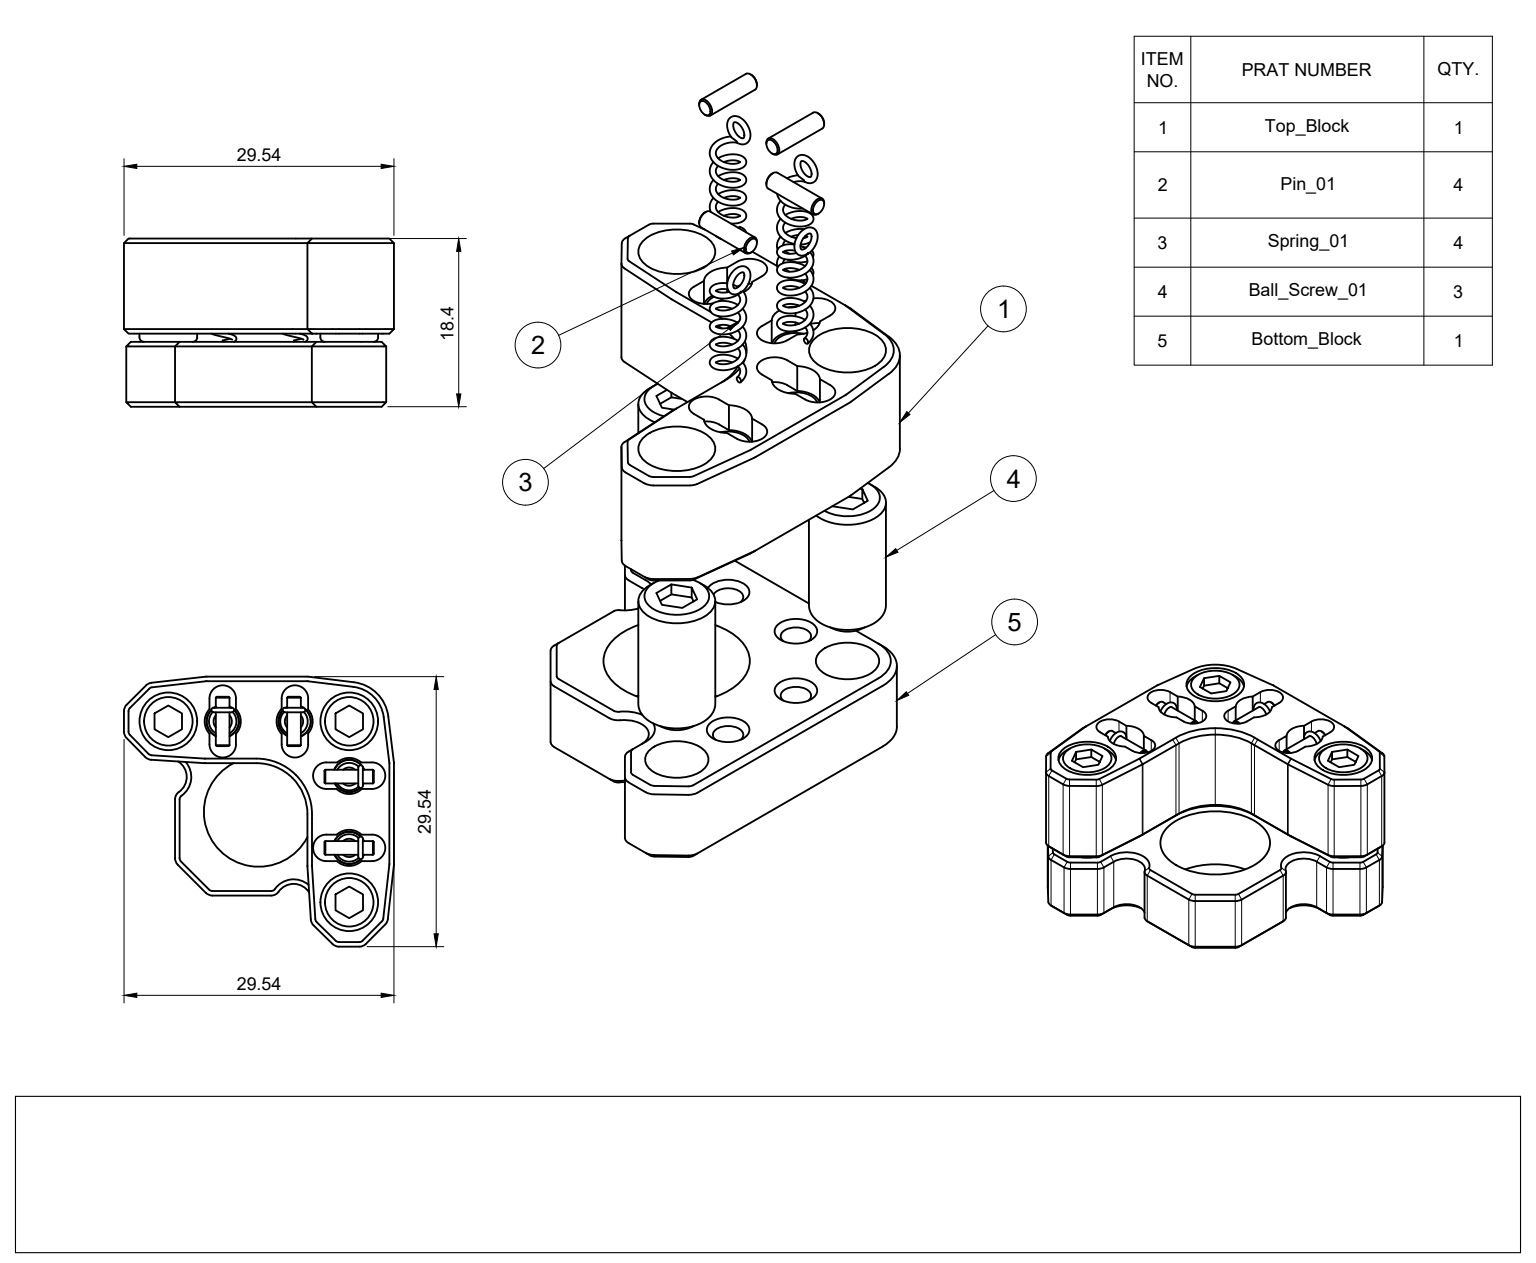
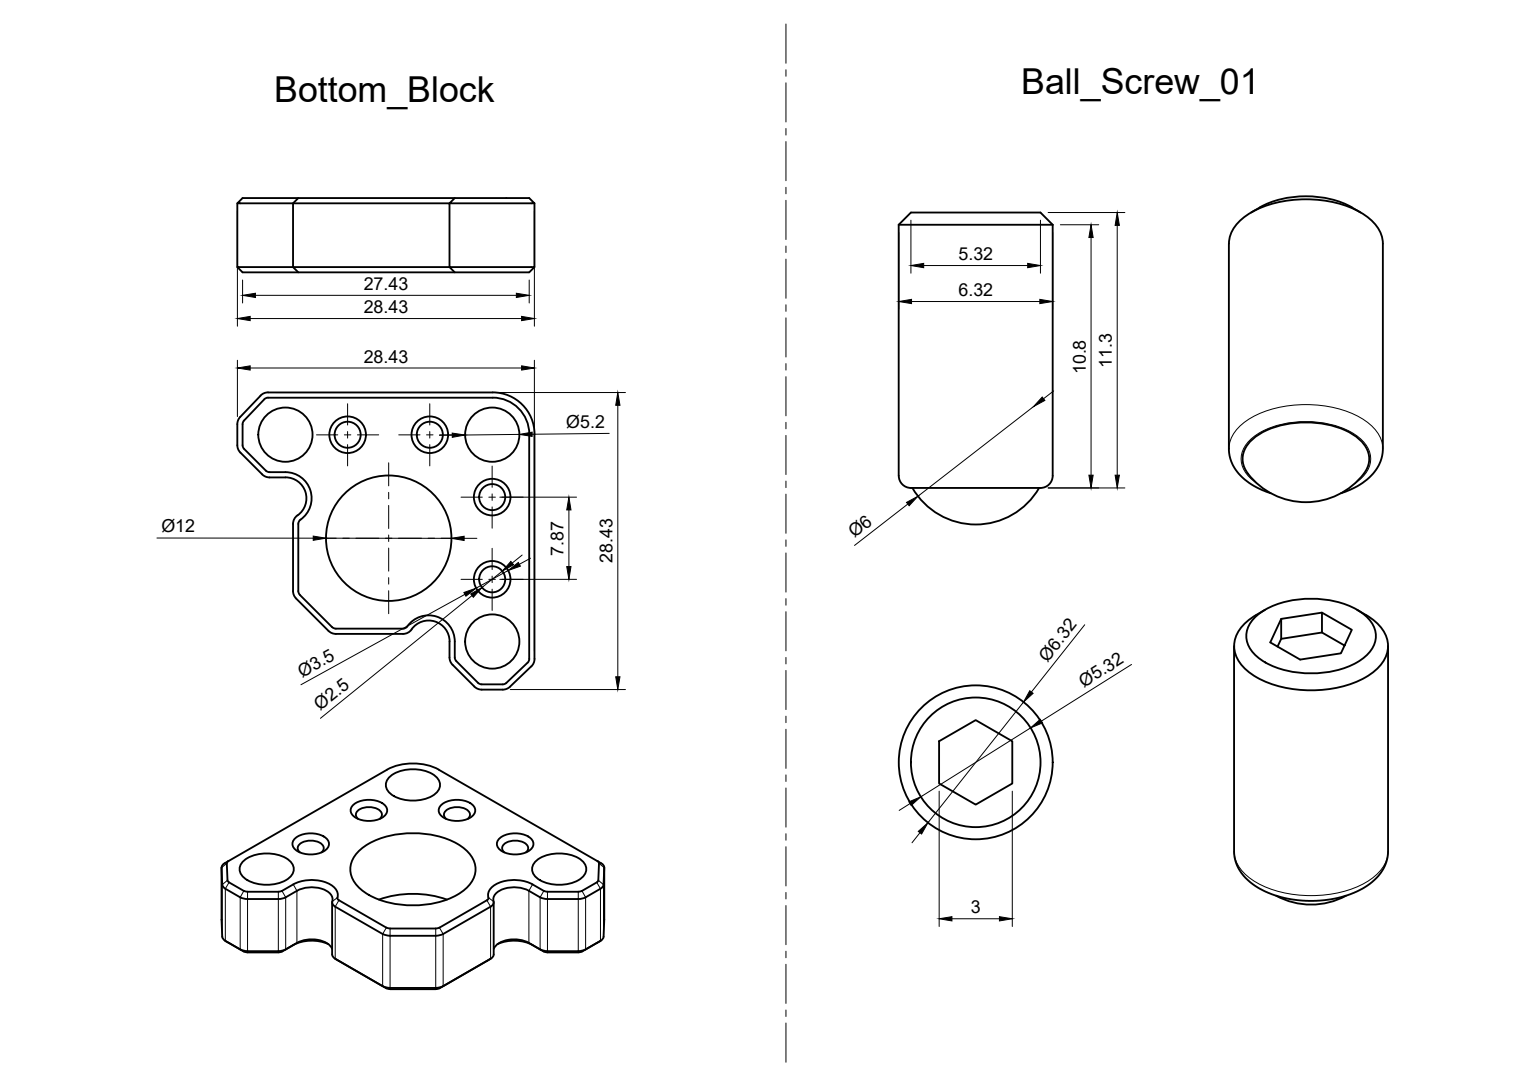
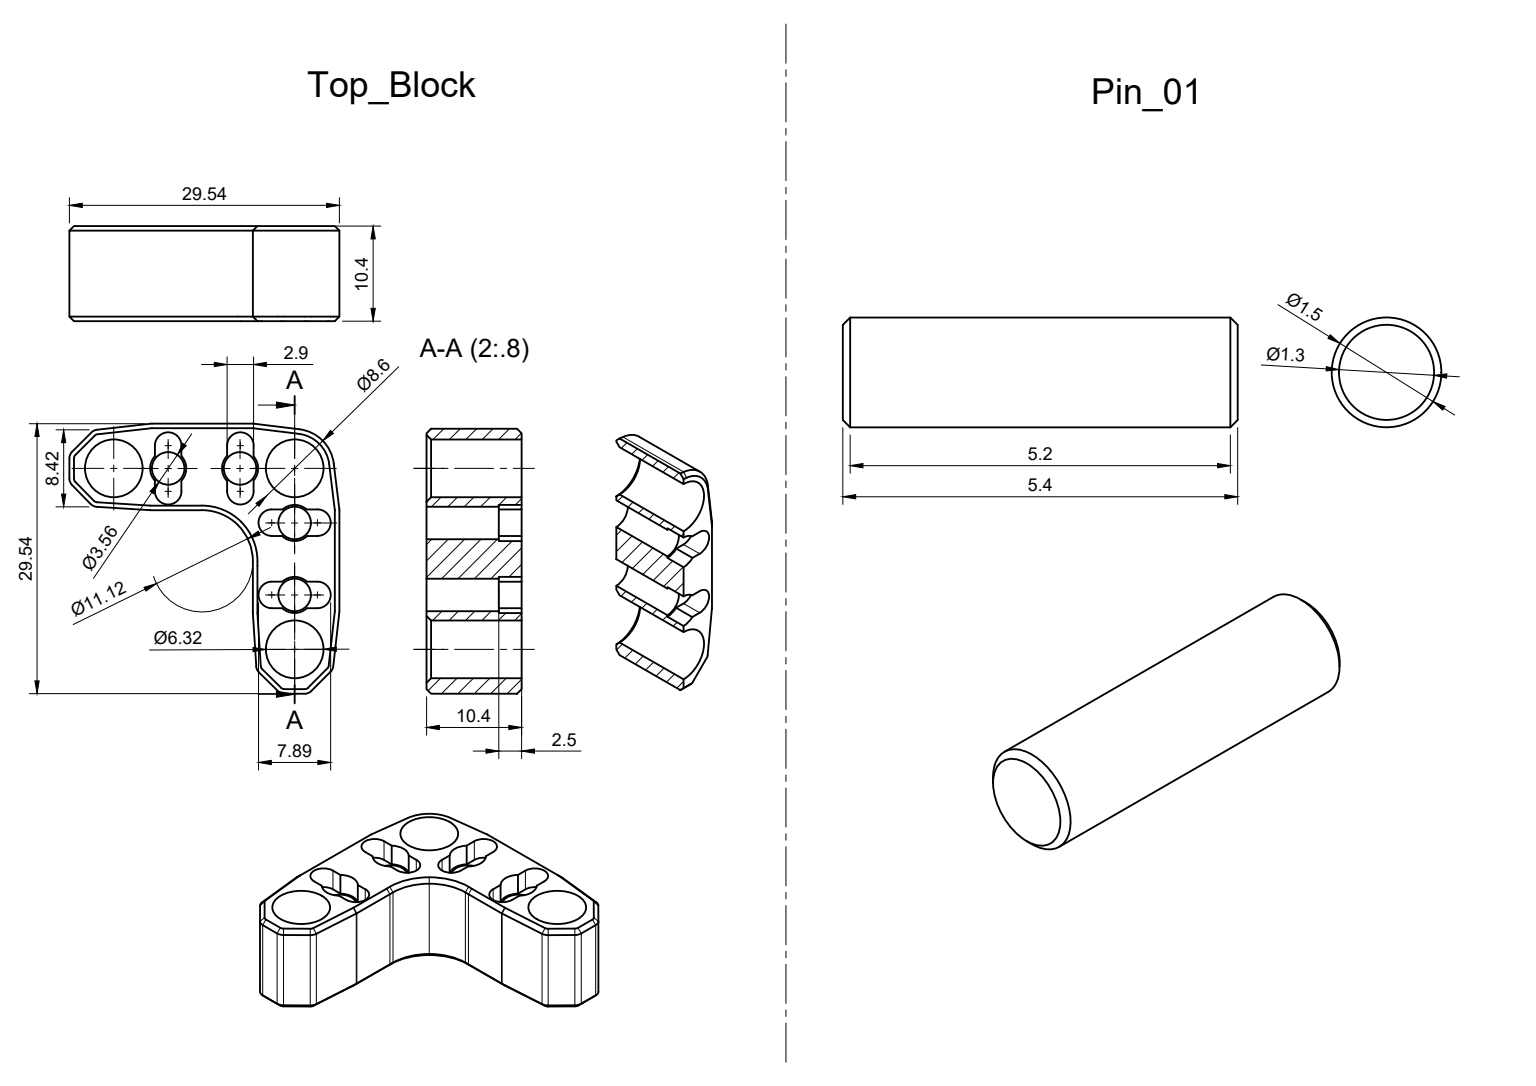
ISO-10303-21;
HEADER;
/* Generated by software containing ST-Developer
 * from STEP Tools, Inc. (www.steptools.com) 
 */

FILE_DESCRIPTION(
/* description */ (''),
/* implementation_level */ '2;1');

FILE_NAME(
/* name */ 'MAS-280',
/* time_stamp */ '2026-10-23T17:00:58+06:00',
/* author */ (''),
/* organization */ (''),
/* preprocessor_version */ 'ST-DEVELOPER v20.2',
/* originating_system */ 'Autodesk Translation Framework v15.15.0.0',
/* authorisation */ '');

FILE_SCHEMA (('AUTOMOTIVE_DESIGN { 1 0 10303 214 3 1 1 }'));
ENDSEC;

DATA;
#10=MECHANICAL_DESIGN_GEOMETRIC_PRESENTATION_REPRESENTATION('',(#106,#107,
#108,#109,#110,#111,#112,#113,#114,#115,#116,#117,#118),#11385);
#11=ITEM_DEFINED_TRANSFORMATION($,$,#5500,#6097);
#12=ITEM_DEFINED_TRANSFORMATION($,$,#5779,#6098);
#13=ITEM_DEFINED_TRANSFORMATION($,$,#5789,#6099);
#14=ITEM_DEFINED_TRANSFORMATION($,$,#5796,#6100);
#15=ITEM_DEFINED_TRANSFORMATION($,$,#5817,#6101);
#16=ITEM_DEFINED_TRANSFORMATION($,$,#6004,#6102);
#17=ITEM_DEFINED_TRANSFORMATION($,$,#6014,#6103);
#18=ITEM_DEFINED_TRANSFORMATION($,$,#6035,#6104);
#19=ITEM_DEFINED_TRANSFORMATION($,$,#6042,#6105);
#20=ITEM_DEFINED_TRANSFORMATION($,$,#6049,#6106);
#21=ITEM_DEFINED_TRANSFORMATION($,$,#6059,#6107);
#22=ITEM_DEFINED_TRANSFORMATION($,$,#6066,#6108);
#23=ITEM_DEFINED_TRANSFORMATION($,$,#6076,#6109);
#24=(
REPRESENTATION_RELATIONSHIP($,$,#11432,#11431)
REPRESENTATION_RELATIONSHIP_WITH_TRANSFORMATION(#11)
SHAPE_REPRESENTATION_RELATIONSHIP()
);
#25=(
REPRESENTATION_RELATIONSHIP($,$,#11433,#11431)
REPRESENTATION_RELATIONSHIP_WITH_TRANSFORMATION(#12)
SHAPE_REPRESENTATION_RELATIONSHIP()
);
#26=(
REPRESENTATION_RELATIONSHIP($,$,#11434,#11431)
REPRESENTATION_RELATIONSHIP_WITH_TRANSFORMATION(#13)
SHAPE_REPRESENTATION_RELATIONSHIP()
);
#27=(
REPRESENTATION_RELATIONSHIP($,$,#11435,#11431)
REPRESENTATION_RELATIONSHIP_WITH_TRANSFORMATION(#14)
SHAPE_REPRESENTATION_RELATIONSHIP()
);
#28=(
REPRESENTATION_RELATIONSHIP($,$,#11436,#11431)
REPRESENTATION_RELATIONSHIP_WITH_TRANSFORMATION(#15)
SHAPE_REPRESENTATION_RELATIONSHIP()
);
#29=(
REPRESENTATION_RELATIONSHIP($,$,#11437,#11431)
REPRESENTATION_RELATIONSHIP_WITH_TRANSFORMATION(#16)
SHAPE_REPRESENTATION_RELATIONSHIP()
);
#30=(
REPRESENTATION_RELATIONSHIP($,$,#11438,#11431)
REPRESENTATION_RELATIONSHIP_WITH_TRANSFORMATION(#17)
SHAPE_REPRESENTATION_RELATIONSHIP()
);
#31=(
REPRESENTATION_RELATIONSHIP($,$,#11439,#11431)
REPRESENTATION_RELATIONSHIP_WITH_TRANSFORMATION(#18)
SHAPE_REPRESENTATION_RELATIONSHIP()
);
#32=(
REPRESENTATION_RELATIONSHIP($,$,#11440,#11431)
REPRESENTATION_RELATIONSHIP_WITH_TRANSFORMATION(#19)
SHAPE_REPRESENTATION_RELATIONSHIP()
);
#33=(
REPRESENTATION_RELATIONSHIP($,$,#11441,#11431)
REPRESENTATION_RELATIONSHIP_WITH_TRANSFORMATION(#20)
SHAPE_REPRESENTATION_RELATIONSHIP()
);
#34=(
REPRESENTATION_RELATIONSHIP($,$,#11442,#11431)
REPRESENTATION_RELATIONSHIP_WITH_TRANSFORMATION(#21)
SHAPE_REPRESENTATION_RELATIONSHIP()
);
#35=(
REPRESENTATION_RELATIONSHIP($,$,#11443,#11431)
REPRESENTATION_RELATIONSHIP_WITH_TRANSFORMATION(#22)
SHAPE_REPRESENTATION_RELATIONSHIP()
);
#36=(
REPRESENTATION_RELATIONSHIP($,$,#11444,#11431)
REPRESENTATION_RELATIONSHIP_WITH_TRANSFORMATION(#23)
SHAPE_REPRESENTATION_RELATIONSHIP()
);
#37=CONTEXT_DEPENDENT_SHAPE_REPRESENTATION(#24,#11418);
#38=CONTEXT_DEPENDENT_SHAPE_REPRESENTATION(#25,#11419);
#39=CONTEXT_DEPENDENT_SHAPE_REPRESENTATION(#26,#11420);
#40=CONTEXT_DEPENDENT_SHAPE_REPRESENTATION(#27,#11421);
#41=CONTEXT_DEPENDENT_SHAPE_REPRESENTATION(#28,#11422);
#42=CONTEXT_DEPENDENT_SHAPE_REPRESENTATION(#29,#11423);
#43=CONTEXT_DEPENDENT_SHAPE_REPRESENTATION(#30,#11424);
#44=CONTEXT_DEPENDENT_SHAPE_REPRESENTATION(#31,#11425);
#45=CONTEXT_DEPENDENT_SHAPE_REPRESENTATION(#32,#11426);
#46=CONTEXT_DEPENDENT_SHAPE_REPRESENTATION(#33,#11427);
#47=CONTEXT_DEPENDENT_SHAPE_REPRESENTATION(#34,#11428);
#48=CONTEXT_DEPENDENT_SHAPE_REPRESENTATION(#35,#11429);
#49=CONTEXT_DEPENDENT_SHAPE_REPRESENTATION(#36,#11430);
#50=NEXT_ASSEMBLY_USAGE_OCCURRENCE('Top_Block:1','Top_Block:1',
'Top_Block:1',#11446,#11447,'Top_Block:1');
#51=NEXT_ASSEMBLY_USAGE_OCCURRENCE('Pin_01:1','Pin_01:1','Pin_01:1',#11446,
#11448,'Pin_01:1');
#52=NEXT_ASSEMBLY_USAGE_OCCURRENCE('Spring_01:1','Spring_01:1',
'Spring_01:1',#11446,#11449,'Spring_01:1');
#53=NEXT_ASSEMBLY_USAGE_OCCURRENCE('Ball_Screw_01:1','Ball_Screw_01:1',
'Ball_Screw_01:1',#11446,#11450,'Ball_Screw_01:1');
#54=NEXT_ASSEMBLY_USAGE_OCCURRENCE('Bottom_Block:1','Bottom_Block:1',
'Bottom_Block:1',#11446,#11451,'Bottom_Block:1');
#55=NEXT_ASSEMBLY_USAGE_OCCURRENCE('Pin_04:1','Pin_04:1','Pin_04:1',#11446,
#11452,'Pin_04:1');
#56=NEXT_ASSEMBLY_USAGE_OCCURRENCE('Ball_Screw_02:1','Ball_Screw_02:1',
'Ball_Screw_02:1',#11446,#11453,'Ball_Screw_02:1');
#57=NEXT_ASSEMBLY_USAGE_OCCURRENCE('Spring_04:1','Spring_04:1',
'Spring_04:1',#11446,#11454,'Spring_04:1');
#58=NEXT_ASSEMBLY_USAGE_OCCURRENCE('Spring_02:1','Spring_02:1',
'Spring_02:1',#11446,#11455,'Spring_02:1');
#59=NEXT_ASSEMBLY_USAGE_OCCURRENCE('Pin_03:1','Pin_03:1','Pin_03:1',#11446,
#11456,'Pin_03:1');
#60=NEXT_ASSEMBLY_USAGE_OCCURRENCE('Spring_03:1','Spring_03:1',
'Spring_03:1',#11446,#11457,'Spring_03:1');
#61=NEXT_ASSEMBLY_USAGE_OCCURRENCE('Pin_02:1','Pin_02:1','Pin_02:1',#11446,
#11458,'Pin_02:1');
#62=NEXT_ASSEMBLY_USAGE_OCCURRENCE('Ball_Screw_03:1','Ball_Screw_03:1',
'Ball_Screw_03:1',#11446,#11459,'Ball_Screw_03:1');
#63=SPHERICAL_SURFACE('',#5797,3.);
#64=SPHERICAL_SURFACE('',#5818,3.);
#65=SPHERICAL_SURFACE('',#5844,3.);
#66=SPHERICAL_SURFACE('',#5846,3.);
#67=SPHERICAL_SURFACE('',#6015,3.);
#68=SPHERICAL_SURFACE('',#6077,3.);
#69=B_SPLINE_SURFACE_WITH_KNOTS('',3,3,((#8625,#8626,#8627,#8628,#8629,
#8630,#8631,#8632,#8633,#8634,#8635,#8636,#8637,#8638,#8639,#8640,#8641,
#8642,#8643,#8644,#8645,#8646,#8647,#8648,#8649,#8650,#8651,#8652,#8653,
#8654,#8655,#8656,#8657,#8658,#8659,#8660,#8661),(#8662,#8663,#8664,#8665,
#8666,#8667,#8668,#8669,#8670,#8671,#8672,#8673,#8674,#8675,#8676,#8677,
#8678,#8679,#8680,#8681,#8682,#8683,#8684,#8685,#8686,#8687,#8688,#8689,
#8690,#8691,#8692,#8693,#8694,#8695,#8696,#8697,#8698),(#8699,#8700,#8701,
#8702,#8703,#8704,#8705,#8706,#8707,#8708,#8709,#8710,#8711,#8712,#8713,
#8714,#8715,#8716,#8717,#8718,#8719,#8720,#8721,#8722,#8723,#8724,#8725,
#8726,#8727,#8728,#8729,#8730,#8731,#8732,#8733,#8734,#8735),(#8736,#8737,
#8738,#8739,#8740,#8741,#8742,#8743,#8744,#8745,#8746,#8747,#8748,#8749,
#8750,#8751,#8752,#8753,#8754,#8755,#8756,#8757,#8758,#8759,#8760,#8761,
#8762,#8763,#8764,#8765,#8766,#8767,#8768,#8769,#8770,#8771,#8772),(#8773,
#8774,#8775,#8776,#8777,#8778,#8779,#8780,#8781,#8782,#8783,#8784,#8785,
#8786,#8787,#8788,#8789,#8790,#8791,#8792,#8793,#8794,#8795,#8796,#8797,
#8798,#8799,#8800,#8801,#8802,#8803,#8804,#8805,#8806,#8807,#8808,#8809),
(#8810,#8811,#8812,#8813,#8814,#8815,#8816,#8817,#8818,#8819,#8820,#8821,
#8822,#8823,#8824,#8825,#8826,#8827,#8828,#8829,#8830,#8831,#8832,#8833,
#8834,#8835,#8836,#8837,#8838,#8839,#8840,#8841,#8842,#8843,#8844,#8845,
#8846),(#8847,#8848,#8849,#8850,#8851,#8852,#8853,#8854,#8855,#8856,#8857,
#8858,#8859,#8860,#8861,#8862,#8863,#8864,#8865,#8866,#8867,#8868,#8869,
#8870,#8871,#8872,#8873,#8874,#8875,#8876,#8877,#8878,#8879,#8880,#8881,
#8882,#8883),(#8884,#8885,#8886,#8887,#8888,#8889,#8890,#8891,#8892,#8893,
#8894,#8895,#8896,#8897,#8898,#8899,#8900,#8901,#8902,#8903,#8904,#8905,
#8906,#8907,#8908,#8909,#8910,#8911,#8912,#8913,#8914,#8915,#8916,#8917,
#8918,#8919,#8920),(#8921,#8922,#8923,#8924,#8925,#8926,#8927,#8928,#8929,
#8930,#8931,#8932,#8933,#8934,#8935,#8936,#8937,#8938,#8939,#8940,#8941,
#8942,#8943,#8944,#8945,#8946,#8947,#8948,#8949,#8950,#8951,#8952,#8953,
#8954,#8955,#8956,#8957),(#8958,#8959,#8960,#8961,#8962,#8963,#8964,#8965,
#8966,#8967,#8968,#8969,#8970,#8971,#8972,#8973,#8974,#8975,#8976,#8977,
#8978,#8979,#8980,#8981,#8982,#8983,#8984,#8985,#8986,#8987,#8988,#8989,
#8990,#8991,#8992,#8993,#8994),(#8995,#8996,#8997,#8998,#8999,#9000,#9001,
#9002,#9003,#9004,#9005,#9006,#9007,#9008,#9009,#9010,#9011,#9012,#9013,
#9014,#9015,#9016,#9017,#9018,#9019,#9020,#9021,#9022,#9023,#9024,#9025,
#9026,#9027,#9028,#9029,#9030,#9031),(#9032,#9033,#9034,#9035,#9036,#9037,
#9038,#9039,#9040,#9041,#9042,#9043,#9044,#9045,#9046,#9047,#9048,#9049,
#9050,#9051,#9052,#9053,#9054,#9055,#9056,#9057,#9058,#9059,#9060,#9061,
#9062,#9063,#9064,#9065,#9066,#9067,#9068)),.UNSPECIFIED.,.T.,.F.,.F.,(4,
1,1,1,1,1,1,1,1,4),(4,1,1,1,1,1,1,1,1,1,1,1,1,1,1,1,1,1,1,1,1,1,1,1,1,1,
1,1,1,1,1,1,1,1,4),(-3.14159265358979,-2.46839422782055,-2.24399475256414,
-1.79519580205131,-1.12199737628207,-0.448798950512828,0.448798950512828,
1.34639685153848,2.24399475256414,3.14159265358979),(0.,0.490873852123405,
0.98174770424681,1.96349540849362,2.94524311274043,3.92699081698724,4.90873852123405,
5.89048622548086,6.87223392972767,7.85398163397448,8.83572933822129,9.8174770424681,
10.7992247467149,11.7809724509617,12.7627201552085,13.7444678594553,14.7262155637022,
15.707963267949,16.6897109721958,17.6714586764426,18.6532063806894,19.6349540849362,
20.616701789183,21.5984494934298,22.5801971976766,23.5619449019234,24.5436926061703,
25.5254403104171,26.5071880146639,27.4889357189107,28.4706834231575,29.4524311274043,
30.4341788316511,30.9250526837745,31.4159265358979),.UNSPECIFIED.);
#70=B_SPLINE_SURFACE_WITH_KNOTS('',3,3,((#9768,#9769,#9770,#9771,#9772,
#9773,#9774,#9775,#9776,#9777,#9778,#9779,#9780,#9781,#9782,#9783,#9784,
#9785,#9786,#9787,#9788,#9789,#9790,#9791,#9792,#9793,#9794,#9795,#9796,
#9797,#9798,#9799,#9800,#9801,#9802,#9803,#9804),(#9805,#9806,#9807,#9808,
#9809,#9810,#9811,#9812,#9813,#9814,#9815,#9816,#9817,#9818,#9819,#9820,
#9821,#9822,#9823,#9824,#9825,#9826,#9827,#9828,#9829,#9830,#9831,#9832,
#9833,#9834,#9835,#9836,#9837,#9838,#9839,#9840,#9841),(#9842,#9843,#9844,
#9845,#9846,#9847,#9848,#9849,#9850,#9851,#9852,#9853,#9854,#9855,#9856,
#9857,#9858,#9859,#9860,#9861,#9862,#9863,#9864,#9865,#9866,#9867,#9868,
#9869,#9870,#9871,#9872,#9873,#9874,#9875,#9876,#9877,#9878),(#9879,#9880,
#9881,#9882,#9883,#9884,#9885,#9886,#9887,#9888,#9889,#9890,#9891,#9892,
#9893,#9894,#9895,#9896,#9897,#9898,#9899,#9900,#9901,#9902,#9903,#9904,
#9905,#9906,#9907,#9908,#9909,#9910,#9911,#9912,#9913,#9914,#9915),(#9916,
#9917,#9918,#9919,#9920,#9921,#9922,#9923,#9924,#9925,#9926,#9927,#9928,
#9929,#9930,#9931,#9932,#9933,#9934,#9935,#9936,#9937,#9938,#9939,#9940,
#9941,#9942,#9943,#9944,#9945,#9946,#9947,#9948,#9949,#9950,#9951,#9952),
(#9953,#9954,#9955,#9956,#9957,#9958,#9959,#9960,#9961,#9962,#9963,#9964,
#9965,#9966,#9967,#9968,#9969,#9970,#9971,#9972,#9973,#9974,#9975,#9976,
#9977,#9978,#9979,#9980,#9981,#9982,#9983,#9984,#9985,#9986,#9987,#9988,
#9989),(#9990,#9991,#9992,#9993,#9994,#9995,#9996,#9997,#9998,#9999,#10000,
#10001,#10002,#10003,#10004,#10005,#10006,#10007,#10008,#10009,#10010,#10011,
#10012,#10013,#10014,#10015,#10016,#10017,#10018,#10019,#10020,#10021,#10022,
#10023,#10024,#10025,#10026),(#10027,#10028,#10029,#10030,#10031,#10032,
#10033,#10034,#10035,#10036,#10037,#10038,#10039,#10040,#10041,#10042,#10043,
#10044,#10045,#10046,#10047,#10048,#10049,#10050,#10051,#10052,#10053,#10054,
#10055,#10056,#10057,#10058,#10059,#10060,#10061,#10062,#10063),(#10064,
#10065,#10066,#10067,#10068,#10069,#10070,#10071,#10072,#10073,#10074,#10075,
#10076,#10077,#10078,#10079,#10080,#10081,#10082,#10083,#10084,#10085,#10086,
#10087,#10088,#10089,#10090,#10091,#10092,#10093,#10094,#10095,#10096,#10097,
#10098,#10099,#10100),(#10101,#10102,#10103,#10104,#10105,#10106,#10107,
#10108,#10109,#10110,#10111,#10112,#10113,#10114,#10115,#10116,#10117,#10118,
#10119,#10120,#10121,#10122,#10123,#10124,#10125,#10126,#10127,#10128,#10129,
#10130,#10131,#10132,#10133,#10134,#10135,#10136,#10137),(#10138,#10139,
#10140,#10141,#10142,#10143,#10144,#10145,#10146,#10147,#10148,#10149,#10150,
#10151,#10152,#10153,#10154,#10155,#10156,#10157,#10158,#10159,#10160,#10161,
#10162,#10163,#10164,#10165,#10166,#10167,#10168,#10169,#10170,#10171,#10172,
#10173,#10174),(#10175,#10176,#10177,#10178,#10179,#10180,#10181,#10182,
#10183,#10184,#10185,#10186,#10187,#10188,#10189,#10190,#10191,#10192,#10193,
#10194,#10195,#10196,#10197,#10198,#10199,#10200,#10201,#10202,#10203,#10204,
#10205,#10206,#10207,#10208,#10209,#10210,#10211)),.UNSPECIFIED.,.T.,.F.,
 .F.,(4,1,1,1,1,1,1,1,1,4),(4,1,1,1,1,1,1,1,1,1,1,1,1,1,1,1,1,1,1,1,1,1,
1,1,1,1,1,1,1,1,1,1,1,1,4),(-3.14159265358979,-2.46839422782055,-2.24399475256414,
-1.79519580205131,-1.12199737628207,-0.448798950512828,0.448798950512828,
1.34639685153848,2.24399475256414,3.14159265358979),(0.,0.490873852123405,
0.98174770424681,1.96349540849362,2.94524311274043,3.92699081698724,4.90873852123405,
5.89048622548086,6.87223392972767,7.85398163397448,8.83572933822129,9.8174770424681,
10.7992247467149,11.7809724509617,12.7627201552085,13.7444678594553,14.7262155637022,
15.707963267949,16.6897109721958,17.6714586764426,18.6532063806894,19.6349540849362,
20.616701789183,21.5984494934298,22.5801971976766,23.5619449019234,24.5436926061703,
25.5254403104171,26.5071880146639,27.4889357189107,28.4706834231575,29.4524311274043,
30.4341788316511,30.9250526837745,31.4159265358979),.UNSPECIFIED.);
#71=B_SPLINE_SURFACE_WITH_KNOTS('',3,3,((#10304,#10305,#10306,#10307,#10308,
#10309,#10310,#10311,#10312,#10313,#10314,#10315,#10316,#10317,#10318,#10319,
#10320,#10321,#10322,#10323,#10324,#10325,#10326,#10327,#10328,#10329,#10330,
#10331,#10332,#10333,#10334,#10335,#10336,#10337,#10338,#10339,#10340),
(#10341,#10342,#10343,#10344,#10345,#10346,#10347,#10348,#10349,#10350,
#10351,#10352,#10353,#10354,#10355,#10356,#10357,#10358,#10359,#10360,#10361,
#10362,#10363,#10364,#10365,#10366,#10367,#10368,#10369,#10370,#10371,#10372,
#10373,#10374,#10375,#10376,#10377),(#10378,#10379,#10380,#10381,#10382,
#10383,#10384,#10385,#10386,#10387,#10388,#10389,#10390,#10391,#10392,#10393,
#10394,#10395,#10396,#10397,#10398,#10399,#10400,#10401,#10402,#10403,#10404,
#10405,#10406,#10407,#10408,#10409,#10410,#10411,#10412,#10413,#10414),
(#10415,#10416,#10417,#10418,#10419,#10420,#10421,#10422,#10423,#10424,
#10425,#10426,#10427,#10428,#10429,#10430,#10431,#10432,#10433,#10434,#10435,
#10436,#10437,#10438,#10439,#10440,#10441,#10442,#10443,#10444,#10445,#10446,
#10447,#10448,#10449,#10450,#10451),(#10452,#10453,#10454,#10455,#10456,
#10457,#10458,#10459,#10460,#10461,#10462,#10463,#10464,#10465,#10466,#10467,
#10468,#10469,#10470,#10471,#10472,#10473,#10474,#10475,#10476,#10477,#10478,
#10479,#10480,#10481,#10482,#10483,#10484,#10485,#10486,#10487,#10488),
(#10489,#10490,#10491,#10492,#10493,#10494,#10495,#10496,#10497,#10498,
#10499,#10500,#10501,#10502,#10503,#10504,#10505,#10506,#10507,#10508,#10509,
#10510,#10511,#10512,#10513,#10514,#10515,#10516,#10517,#10518,#10519,#10520,
#10521,#10522,#10523,#10524,#10525),(#10526,#10527,#10528,#10529,#10530,
#10531,#10532,#10533,#10534,#10535,#10536,#10537,#10538,#10539,#10540,#10541,
#10542,#10543,#10544,#10545,#10546,#10547,#10548,#10549,#10550,#10551,#10552,
#10553,#10554,#10555,#10556,#10557,#10558,#10559,#10560,#10561,#10562),
(#10563,#10564,#10565,#10566,#10567,#10568,#10569,#10570,#10571,#10572,
#10573,#10574,#10575,#10576,#10577,#10578,#10579,#10580,#10581,#10582,#10583,
#10584,#10585,#10586,#10587,#10588,#10589,#10590,#10591,#10592,#10593,#10594,
#10595,#10596,#10597,#10598,#10599),(#10600,#10601,#10602,#10603,#10604,
#10605,#10606,#10607,#10608,#10609,#10610,#10611,#10612,#10613,#10614,#10615,
#10616,#10617,#10618,#10619,#10620,#10621,#10622,#10623,#10624,#10625,#10626,
#10627,#10628,#10629,#10630,#10631,#10632,#10633,#10634,#10635,#10636),
(#10637,#10638,#10639,#10640,#10641,#10642,#10643,#10644,#10645,#10646,
#10647,#10648,#10649,#10650,#10651,#10652,#10653,#10654,#10655,#10656,#10657,
#10658,#10659,#10660,#10661,#10662,#10663,#10664,#10665,#10666,#10667,#10668,
#10669,#10670,#10671,#10672,#10673),(#10674,#10675,#10676,#10677,#10678,
#10679,#10680,#10681,#10682,#10683,#10684,#10685,#10686,#10687,#10688,#10689,
#10690,#10691,#10692,#10693,#10694,#10695,#10696,#10697,#10698,#10699,#10700,
#10701,#10702,#10703,#10704,#10705,#10706,#10707,#10708,#10709,#10710),
(#10711,#10712,#10713,#10714,#10715,#10716,#10717,#10718,#10719,#10720,
#10721,#10722,#10723,#10724,#10725,#10726,#10727,#10728,#10729,#10730,#10731,
#10732,#10733,#10734,#10735,#10736,#10737,#10738,#10739,#10740,#10741,#10742,
#10743,#10744,#10745,#10746,#10747)),.UNSPECIFIED.,.T.,.F.,.F.,(4,1,1,1,
1,1,1,1,1,4),(4,1,1,1,1,1,1,1,1,1,1,1,1,1,1,1,1,1,1,1,1,1,1,1,1,1,1,1,1,
1,1,1,1,1,4),(-3.14159265358979,-2.46839422782055,-2.24399475256414,-1.79519580205131,
-1.12199737628207,-0.448798950512828,0.448798950512828,1.34639685153848,
2.24399475256414,3.14159265358979),(0.,0.490873852123405,0.98174770424681,
1.96349540849362,2.94524311274043,3.92699081698724,4.90873852123405,5.89048622548086,
6.87223392972767,7.85398163397448,8.83572933822129,9.8174770424681,10.7992247467149,
11.7809724509617,12.7627201552085,13.7444678594553,14.7262155637022,15.707963267949,
16.6897109721958,17.6714586764426,18.6532063806894,19.6349540849362,20.616701789183,
21.5984494934298,22.5801971976766,23.5619449019234,24.5436926061703,25.5254403104171,
26.5071880146639,27.4889357189107,28.4706834231575,29.4524311274043,30.4341788316511,
30.9250526837745,31.4159265358979),.UNSPECIFIED.);
#72=B_SPLINE_SURFACE_WITH_KNOTS('',3,3,((#10857,#10858,#10859,#10860,#10861,
#10862,#10863,#10864,#10865,#10866,#10867,#10868,#10869,#10870,#10871,#10872,
#10873,#10874,#10875,#10876,#10877,#10878,#10879,#10880,#10881,#10882,#10883,
#10884,#10885,#10886,#10887,#10888,#10889,#10890,#10891,#10892,#10893),
(#10894,#10895,#10896,#10897,#10898,#10899,#10900,#10901,#10902,#10903,
#10904,#10905,#10906,#10907,#10908,#10909,#10910,#10911,#10912,#10913,#10914,
#10915,#10916,#10917,#10918,#10919,#10920,#10921,#10922,#10923,#10924,#10925,
#10926,#10927,#10928,#10929,#10930),(#10931,#10932,#10933,#10934,#10935,
#10936,#10937,#10938,#10939,#10940,#10941,#10942,#10943,#10944,#10945,#10946,
#10947,#10948,#10949,#10950,#10951,#10952,#10953,#10954,#10955,#10956,#10957,
#10958,#10959,#10960,#10961,#10962,#10963,#10964,#10965,#10966,#10967),
(#10968,#10969,#10970,#10971,#10972,#10973,#10974,#10975,#10976,#10977,
#10978,#10979,#10980,#10981,#10982,#10983,#10984,#10985,#10986,#10987,#10988,
#10989,#10990,#10991,#10992,#10993,#10994,#10995,#10996,#10997,#10998,#10999,
#11000,#11001,#11002,#11003,#11004),(#11005,#11006,#11007,#11008,#11009,
#11010,#11011,#11012,#11013,#11014,#11015,#11016,#11017,#11018,#11019,#11020,
#11021,#11022,#11023,#11024,#11025,#11026,#11027,#11028,#11029,#11030,#11031,
#11032,#11033,#11034,#11035,#11036,#11037,#11038,#11039,#11040,#11041),
(#11042,#11043,#11044,#11045,#11046,#11047,#11048,#11049,#11050,#11051,
#11052,#11053,#11054,#11055,#11056,#11057,#11058,#11059,#11060,#11061,#11062,
#11063,#11064,#11065,#11066,#11067,#11068,#11069,#11070,#11071,#11072,#11073,
#11074,#11075,#11076,#11077,#11078),(#11079,#11080,#11081,#11082,#11083,
#11084,#11085,#11086,#11087,#11088,#11089,#11090,#11091,#11092,#11093,#11094,
#11095,#11096,#11097,#11098,#11099,#11100,#11101,#11102,#11103,#11104,#11105,
#11106,#11107,#11108,#11109,#11110,#11111,#11112,#11113,#11114,#11115),
(#11116,#11117,#11118,#11119,#11120,#11121,#11122,#11123,#11124,#11125,
#11126,#11127,#11128,#11129,#11130,#11131,#11132,#11133,#11134,#11135,#11136,
#11137,#11138,#11139,#11140,#11141,#11142,#11143,#11144,#11145,#11146,#11147,
#11148,#11149,#11150,#11151,#11152),(#11153,#11154,#11155,#11156,#11157,
#11158,#11159,#11160,#11161,#11162,#11163,#11164,#11165,#11166,#11167,#11168,
#11169,#11170,#11171,#11172,#11173,#11174,#11175,#11176,#11177,#11178,#11179,
#11180,#11181,#11182,#11183,#11184,#11185,#11186,#11187,#11188,#11189),
(#11190,#11191,#11192,#11193,#11194,#11195,#11196,#11197,#11198,#11199,
#11200,#11201,#11202,#11203,#11204,#11205,#11206,#11207,#11208,#11209,#11210,
#11211,#11212,#11213,#11214,#11215,#11216,#11217,#11218,#11219,#11220,#11221,
#11222,#11223,#11224,#11225,#11226)),.UNSPECIFIED.,.T.,.F.,.F.,(4,1,1,1,
1,1,1,4),(4,1,1,1,1,1,1,1,1,1,1,1,1,1,1,1,1,1,1,1,1,1,1,1,1,1,1,1,1,1,1,
1,1,1,4),(-3.14159265358979,-2.24399475256414,-1.34639685153848,-0.448798950512828,
0.448798950512828,1.34639685153848,2.24399475256414,3.14159265358979),(0.,
0.490873852123405,0.98174770424681,1.96349540849362,2.94524311274043,3.92699081698724,
4.90873852123405,5.89048622548086,6.87223392972767,7.85398163397448,8.83572933822129,
9.8174770424681,10.7992247467149,11.7809724509617,12.7627201552085,13.7444678594553,
14.7262155637022,15.707963267949,16.6897109721958,17.6714586764426,18.6532063806894,
19.6349540849362,20.616701789183,21.5984494934298,22.5801971976766,23.5619449019234,
24.5436926061703,25.5254403104171,26.5071880146639,27.4889357189107,28.4706834231575,
29.4524311274043,30.4341788316511,30.9250526837745,31.4159265358979),
 .UNSPECIFIED.);
#73=TOROIDAL_SURFACE('',#5790,1.,0.25);
#74=TOROIDAL_SURFACE('',#5800,2.65761552865316,0.5);
#75=TOROIDAL_SURFACE('',#6018,2.65761552865316,0.5);
#76=TOROIDAL_SURFACE('',#6036,1.,0.25);
#77=TOROIDAL_SURFACE('',#6043,1.,0.25);
#78=TOROIDAL_SURFACE('',#6060,1.,0.25);
#79=TOROIDAL_SURFACE('',#6080,2.65761552865316,0.5);
#80=SHAPE_REPRESENTATION_RELATIONSHIP('SRR','None',#11432,#93);
#81=SHAPE_REPRESENTATION_RELATIONSHIP('SRR','None',#11433,#94);
#82=SHAPE_REPRESENTATION_RELATIONSHIP('SRR','None',#11434,#95);
#83=SHAPE_REPRESENTATION_RELATIONSHIP('SRR','None',#11435,#96);
#84=SHAPE_REPRESENTATION_RELATIONSHIP('SRR','None',#11436,#97);
#85=SHAPE_REPRESENTATION_RELATIONSHIP('SRR','None',#11437,#98);
#86=SHAPE_REPRESENTATION_RELATIONSHIP('SRR','None',#11438,#99);
#87=SHAPE_REPRESENTATION_RELATIONSHIP('SRR','None',#11439,#100);
#88=SHAPE_REPRESENTATION_RELATIONSHIP('SRR','None',#11440,#101);
#89=SHAPE_REPRESENTATION_RELATIONSHIP('SRR','None',#11441,#102);
#90=SHAPE_REPRESENTATION_RELATIONSHIP('SRR','None',#11442,#103);
#91=SHAPE_REPRESENTATION_RELATIONSHIP('SRR','None',#11443,#104);
#92=SHAPE_REPRESENTATION_RELATIONSHIP('SRR','None',#11444,#105);
#93=ADVANCED_BREP_SHAPE_REPRESENTATION('',(#119),#11372);
#94=ADVANCED_BREP_SHAPE_REPRESENTATION('',(#120),#11373);
#95=ADVANCED_BREP_SHAPE_REPRESENTATION('',(#121),#11374);
#96=ADVANCED_BREP_SHAPE_REPRESENTATION('',(#122),#11375);
#97=ADVANCED_BREP_SHAPE_REPRESENTATION('',(#123),#11376);
#98=ADVANCED_BREP_SHAPE_REPRESENTATION('',(#124),#11377);
#99=ADVANCED_BREP_SHAPE_REPRESENTATION('',(#125),#11378);
#100=ADVANCED_BREP_SHAPE_REPRESENTATION('',(#126),#11379);
#101=ADVANCED_BREP_SHAPE_REPRESENTATION('',(#127),#11380);
#102=ADVANCED_BREP_SHAPE_REPRESENTATION('',(#128),#11381);
#103=ADVANCED_BREP_SHAPE_REPRESENTATION('',(#129),#11382);
#104=ADVANCED_BREP_SHAPE_REPRESENTATION('',(#130),#11383);
#105=ADVANCED_BREP_SHAPE_REPRESENTATION('',(#131),#11384);
#106=STYLED_ITEM('',(#11546),#119);
#107=STYLED_ITEM('',(#11567),#120);
#108=STYLED_ITEM('',(#11567),#121);
#109=STYLED_ITEM('',(#11574),#122);
#110=STYLED_ITEM('',(#11546),#123);
#111=STYLED_ITEM('',(#11567),#124);
#112=STYLED_ITEM('',(#11574),#125);
#113=STYLED_ITEM('',(#11567),#126);
#114=STYLED_ITEM('',(#11567),#127);
#115=STYLED_ITEM('',(#11567),#128);
#116=STYLED_ITEM('',(#11567),#129);
#117=STYLED_ITEM('',(#11567),#130);
#118=STYLED_ITEM('',(#11574),#131);
#119=MANIFOLD_SOLID_BREP('Top_Block',#5342);
#120=MANIFOLD_SOLID_BREP('Pin_01',#5343);
#121=MANIFOLD_SOLID_BREP('Spring_01',#5344);
#122=MANIFOLD_SOLID_BREP('Ball_Screw_01',#5345);
#123=MANIFOLD_SOLID_BREP('Bottom_Block',#5346);
#124=MANIFOLD_SOLID_BREP('Pin_04',#5347);
#125=MANIFOLD_SOLID_BREP('Ball_Screw_02',#5348);
#126=MANIFOLD_SOLID_BREP('Spring_04',#5349);
#127=MANIFOLD_SOLID_BREP('Spring_02',#5350);
#128=MANIFOLD_SOLID_BREP('Pin_03',#5351);
#129=MANIFOLD_SOLID_BREP('Spring_03',#5352);
#130=MANIFOLD_SOLID_BREP('Pin_02',#5353);
#131=MANIFOLD_SOLID_BREP('Ball_Screw_03',#5354);
#132=FACE_BOUND('',#1018,.T.);
#133=FACE_BOUND('',#1019,.T.);
#134=FACE_BOUND('',#1020,.T.);
#135=FACE_BOUND('',#1021,.T.);
#136=FACE_BOUND('',#1022,.T.);
#137=FACE_BOUND('',#1023,.T.);
#138=FACE_BOUND('',#1024,.T.);
#139=FACE_BOUND('',#1077,.T.);
#140=FACE_BOUND('',#1078,.T.);
#141=FACE_BOUND('',#1079,.T.);
#142=FACE_BOUND('',#1080,.T.);
#143=FACE_BOUND('',#1081,.T.);
#144=FACE_BOUND('',#1082,.T.);
#145=FACE_BOUND('',#1083,.T.);
#146=FACE_BOUND('',#1085,.T.);
#147=FACE_BOUND('',#1087,.T.);
#148=FACE_BOUND('',#1089,.T.);
#149=FACE_BOUND('',#1091,.T.);
#150=FACE_BOUND('',#1107,.T.);
#151=FACE_BOUND('',#1114,.T.);
#152=FACE_BOUND('',#1124,.T.);
#153=FACE_BOUND('',#1127,.T.);
#154=FACE_BOUND('',#1128,.T.);
#155=FACE_BOUND('',#1129,.T.);
#156=FACE_BOUND('',#1130,.T.);
#157=FACE_BOUND('',#1131,.T.);
#158=FACE_BOUND('',#1132,.T.);
#159=FACE_BOUND('',#1133,.T.);
#160=FACE_BOUND('',#1134,.T.);
#161=FACE_BOUND('',#1147,.T.);
#162=FACE_BOUND('',#1148,.T.);
#163=FACE_BOUND('',#1149,.T.);
#164=FACE_BOUND('',#1150,.T.);
#165=FACE_BOUND('',#1151,.T.);
#166=FACE_BOUND('',#1249,.T.);
#167=FACE_BOUND('',#1259,.T.);
#168=FACE_BOUND('',#1261,.T.);
#169=FACE_BOUND('',#1265,.T.);
#170=FACE_BOUND('',#1274,.T.);
#171=FACE_BOUND('',#1286,.T.);
#172=FACE_BOUND('',#1296,.T.);
#173=B_SPLINE_CURVE_WITH_KNOTS('',3,(#8003,#8004,#8005,#8006,#8007,#8008,
#8009,#8010,#8011,#8012),.UNSPECIFIED.,.F.,.F.,(4,2,2,2,4),(0.,0.0304288686048288,
0.0608577372096576,0.0912866058144864,0.121715474419315),.UNSPECIFIED.);
#174=B_SPLINE_CURVE_WITH_KNOTS('',3,(#8306,#8307,#8308,#8309,#8310,#8311,
#8312,#8313,#8314,#8315),.UNSPECIFIED.,.F.,.F.,(4,2,2,2,4),(0.,0.0304288686048287,
0.0608577372096575,0.0912866058144862,0.121715474419315),.UNSPECIFIED.);
#175=B_SPLINE_CURVE_WITH_KNOTS('',3,(#8581,#8582,#8583,#8584,#8585,#8586,
#8587,#8588,#8589,#8590,#8591,#8592,#8593,#8594,#8595,#8596,#8597,#8598,
#8599,#8600,#8601,#8602,#8603,#8604,#8605,#8606,#8607,#8608,#8609,#8610,
#8611,#8612,#8613,#8614,#8615,#8616,#8617,#8618,#8619,#8620,#8621,#8622,
#8623,#8624),.UNSPECIFIED.,.F.,.F.,(4,2,2,2,2,2,2,2,2,2,2,2,2,2,2,2,2,2,
2,2,2,4),(-0.181685657499379,-0.180553745361431,-0.170622434730818,-0.170447684206912,
-0.167737370927117,-0.166612489538818,-0.16575101153334,-0.16478662015514,
-0.16342132279605,-0.160072321773434,-0.151029759575816,-0.145020173168477,
-0.126301129887337,-0.111561605759352,-0.101015311157688,-0.0928919097586381,
-0.0856896815461206,-0.0776947291824182,-0.0660486167614411,-0.0443043011100664,
0.,0.000811103137473634),.UNSPECIFIED.);
#176=B_SPLINE_CURVE_WITH_KNOTS('',3,(#9070,#9071,#9072,#9073,#9074,#9075,
#9076,#9077,#9078,#9079,#9080,#9081,#9082,#9083,#9084,#9085,#9086,#9087,
#9088,#9089,#9090,#9091,#9092,#9093,#9094,#9095,#9096,#9097,#9098,#9099,
#9100,#9101,#9102,#9103,#9104,#9105,#9106),.UNSPECIFIED.,.F.,.F.,(4,1,1,
1,1,1,1,1,1,1,1,1,1,1,1,1,1,1,1,1,1,1,1,1,1,1,1,1,1,1,1,1,1,1,4),(0.,0.490873852123405,
0.98174770424681,1.96349540849362,2.94524311274043,3.92699081698724,4.90873852123405,
5.89048622548086,6.87223392972767,7.85398163397448,8.83572933822129,9.8174770424681,
10.7992247467149,11.7809724509617,12.7627201552085,13.7444678594553,14.7262155637022,
15.707963267949,16.6897109721958,17.6714586764426,18.6532063806894,19.6349540849362,
20.616701789183,21.5984494934298,22.5801971976766,23.5619449019234,24.5436926061703,
25.5254403104171,26.5071880146639,27.4889357189107,28.4706834231575,29.4524311274043,
30.4341788316511,30.9250526837745,31.4159265358979),.UNSPECIFIED.);
#177=B_SPLINE_CURVE_WITH_KNOTS('',3,(#9724,#9725,#9726,#9727,#9728,#9729,
#9730,#9731,#9732,#9733,#9734,#9735,#9736,#9737,#9738,#9739,#9740,#9741,
#9742,#9743,#9744,#9745,#9746,#9747,#9748,#9749,#9750,#9751,#9752,#9753,
#9754,#9755,#9756,#9757,#9758,#9759,#9760,#9761,#9762,#9763,#9764,#9765,
#9766,#9767),.UNSPECIFIED.,.F.,.F.,(4,2,2,2,2,2,2,2,2,2,2,2,2,2,2,2,2,2,
2,2,2,4),(-0.181685657499379,-0.180553745361431,-0.170622434730818,-0.170447684206912,
-0.167737370927117,-0.166612489538818,-0.16575101153334,-0.16478662015514,
-0.16342132279605,-0.160072321773434,-0.151029759575816,-0.145020173168477,
-0.126301129887337,-0.111561605759352,-0.101015311157688,-0.0928919097586381,
-0.0856896815461206,-0.0776947291824182,-0.0660486167614411,-0.0443043011100664,
0.,0.000811103137473634),.UNSPECIFIED.);
#178=B_SPLINE_CURVE_WITH_KNOTS('',3,(#10213,#10214,#10215,#10216,#10217,
#10218,#10219,#10220,#10221,#10222,#10223,#10224,#10225,#10226,#10227,#10228,
#10229,#10230,#10231,#10232,#10233,#10234,#10235,#10236,#10237,#10238,#10239,
#10240,#10241,#10242,#10243,#10244,#10245,#10246,#10247,#10248,#10249),
 .UNSPECIFIED.,.F.,.F.,(4,1,1,1,1,1,1,1,1,1,1,1,1,1,1,1,1,1,1,1,1,1,1,1,
1,1,1,1,1,1,1,1,1,1,4),(0.,0.490873852123405,0.98174770424681,1.96349540849362,
2.94524311274043,3.92699081698724,4.90873852123405,5.89048622548086,6.87223392972767,
7.85398163397448,8.83572933822129,9.8174770424681,10.7992247467149,11.7809724509617,
12.7627201552085,13.7444678594553,14.7262155637022,15.707963267949,16.6897109721958,
17.6714586764426,18.6532063806894,19.6349540849362,20.616701789183,21.5984494934298,
22.5801971976766,23.5619449019234,24.5436926061703,25.5254403104171,26.5071880146639,
27.4889357189107,28.4706834231575,29.4524311274043,30.4341788316511,30.9250526837745,
31.4159265358979),.UNSPECIFIED.);
#179=B_SPLINE_CURVE_WITH_KNOTS('',3,(#10260,#10261,#10262,#10263,#10264,
#10265,#10266,#10267,#10268,#10269,#10270,#10271,#10272,#10273,#10274,#10275,
#10276,#10277,#10278,#10279,#10280,#10281,#10282,#10283,#10284,#10285,#10286,
#10287,#10288,#10289,#10290,#10291,#10292,#10293,#10294,#10295,#10296,#10297,
#10298,#10299,#10300,#10301,#10302,#10303),.UNSPECIFIED.,.F.,.F.,(4,2,2,
2,2,2,2,2,2,2,2,2,2,2,2,2,2,2,2,2,2,4),(-0.181685657499379,-0.180553745361431,
-0.170622434730818,-0.170447684206912,-0.167737370927117,-0.166612489538818,
-0.16575101153334,-0.16478662015514,-0.16342132279605,-0.160072321773434,
-0.151029759575816,-0.145020173168477,-0.126301129887337,-0.111561605759352,
-0.101015311157688,-0.0928919097586381,-0.0856896815461206,-0.0776947291824182,
-0.0660486167614411,-0.0443043011100664,0.,0.000811103137473634),
 .UNSPECIFIED.);
#180=B_SPLINE_CURVE_WITH_KNOTS('',3,(#10749,#10750,#10751,#10752,#10753,
#10754,#10755,#10756,#10757,#10758,#10759,#10760,#10761,#10762,#10763,#10764,
#10765,#10766,#10767,#10768,#10769,#10770,#10771,#10772,#10773,#10774,#10775,
#10776,#10777,#10778,#10779,#10780,#10781,#10782,#10783,#10784,#10785),
 .UNSPECIFIED.,.F.,.F.,(4,1,1,1,1,1,1,1,1,1,1,1,1,1,1,1,1,1,1,1,1,1,1,1,
1,1,1,1,1,1,1,1,1,1,4),(0.,0.490873852123405,0.98174770424681,1.96349540849362,
2.94524311274043,3.92699081698724,4.90873852123405,5.89048622548086,6.87223392972767,
7.85398163397448,8.83572933822129,9.8174770424681,10.7992247467149,11.7809724509617,
12.7627201552085,13.7444678594553,14.7262155637022,15.707963267949,16.6897109721958,
17.6714586764426,18.6532063806894,19.6349540849362,20.616701789183,21.5984494934298,
22.5801971976766,23.5619449019234,24.5436926061703,25.5254403104171,26.5071880146639,
27.4889357189107,28.4706834231575,29.4524311274043,30.4341788316511,30.9250526837745,
31.4159265358979),.UNSPECIFIED.);
#181=B_SPLINE_CURVE_WITH_KNOTS('',3,(#10813,#10814,#10815,#10816,#10817,
#10818,#10819,#10820,#10821,#10822,#10823,#10824,#10825,#10826,#10827,#10828,
#10829,#10830,#10831,#10832,#10833,#10834,#10835,#10836,#10837,#10838,#10839,
#10840,#10841,#10842,#10843,#10844,#10845,#10846,#10847,#10848,#10849,#10850,
#10851,#10852,#10853,#10854,#10855,#10856),.UNSPECIFIED.,.F.,.F.,(4,2,2,
2,2,2,2,2,2,2,2,2,2,2,2,2,2,2,2,2,2,4),(-0.181685657499379,-0.180553745361431,
-0.170622434730818,-0.170447684206912,-0.167737370927117,-0.166612489538818,
-0.16575101153334,-0.16478662015514,-0.16342132279605,-0.160072321773434,
-0.151029759575816,-0.145020173168477,-0.126301129887337,-0.111561605759352,
-0.101015311157688,-0.0928919097586381,-0.0856896815461206,-0.0776947291824182,
-0.0660486167614411,-0.0443043011100664,0.,0.000811103137473634),
 .UNSPECIFIED.);
#182=B_SPLINE_CURVE_WITH_KNOTS('',3,(#11228,#11229,#11230,#11231,#11232,
#11233,#11234,#11235,#11236,#11237,#11238,#11239,#11240,#11241,#11242,#11243,
#11244,#11245,#11246,#11247,#11248,#11249,#11250,#11251,#11252,#11253,#11254,
#11255,#11256,#11257,#11258,#11259,#11260,#11261,#11262,#11263,#11264),
 .UNSPECIFIED.,.F.,.F.,(4,1,1,1,1,1,1,1,1,1,1,1,1,1,1,1,1,1,1,1,1,1,1,1,
1,1,1,1,1,1,1,1,1,1,4),(0.,0.490873852123405,0.98174770424681,1.96349540849362,
2.94524311274043,3.92699081698724,4.90873852123405,5.89048622548086,6.87223392972767,
7.85398163397448,8.83572933822129,9.8174770424681,10.7992247467149,11.7809724509617,
12.7627201552085,13.7444678594553,14.7262155637022,15.707963267949,16.6897109721958,
17.6714586764426,18.6532063806894,19.6349540849362,20.616701789183,21.5984494934298,
22.5801971976766,23.5619449019234,24.5436926061703,25.5254403104171,26.5071880146639,
27.4889357189107,28.4706834231575,29.4524311274043,30.4341788316511,30.9250526837745,
31.4159265358979),.UNSPECIFIED.);
#183=CONICAL_SURFACE('',#5571,5.8095085413358,0.785398163397448);
#184=CONICAL_SURFACE('',#5574,99.75,0.785398163397445);
#185=CONICAL_SURFACE('',#5578,1.25000000000098,0.785398163397449);
#186=CONICAL_SURFACE('',#5582,0.750000000000013,0.785398163397449);
#187=CONICAL_SURFACE('',#5586,0.750000000000014,0.785398163397448);
#188=CONICAL_SURFACE('',#5590,0.749999999999996,0.785398163397449);
#189=CONICAL_SURFACE('',#5594,0.750000000000022,0.785398163397448);
#190=CONICAL_SURFACE('',#5598,1.25000000000025,0.785398163397447);
#191=CONICAL_SURFACE('',#5602,1.25000000000039,0.785398163397448);
#192=CONICAL_SURFACE('',#5606,4.05072977423739,0.785398163397448);
#193=CONICAL_SURFACE('',#5610,1.25000000000039,0.785398163397448);
#194=CONICAL_SURFACE('',#5614,1.25000000000025,0.785398163397447);
#195=CONICAL_SURFACE('',#5618,0.750000000000022,0.785398163397448);
#196=CONICAL_SURFACE('',#5622,0.749999999999996,0.785398163397449);
#197=CONICAL_SURFACE('',#5626,0.750000000000014,0.785398163397448);
#198=CONICAL_SURFACE('',#5630,0.750000000000013,0.785398163397449);
#199=CONICAL_SURFACE('',#5634,1.25000000000098,0.785398163397449);
#200=CONICAL_SURFACE('',#5638,99.75,0.785398163397445);
#201=CONICAL_SURFACE('',#5641,5.8095085413358,0.785398163397447);
#202=CONICAL_SURFACE('',#5678,5.8095085413358,0.785398163397448);
#203=CONICAL_SURFACE('',#5680,99.75,0.785398163397446);
#204=CONICAL_SURFACE('',#5683,1.25000000000098,0.78539816339745);
#205=CONICAL_SURFACE('',#5686,0.750000000000013,0.785398163397449);
#206=CONICAL_SURFACE('',#5689,0.750000000000014,0.785398163397449);
#207=CONICAL_SURFACE('',#5692,0.749999999999996,0.785398163397449);
#208=CONICAL_SURFACE('',#5695,0.750000000000022,0.785398163397448);
#209=CONICAL_SURFACE('',#5698,1.25000000000025,0.785398163397448);
#210=CONICAL_SURFACE('',#5701,1.25000000000039,0.785398163397448);
#211=CONICAL_SURFACE('',#5704,4.05072977423739,0.785398163397448);
#212=CONICAL_SURFACE('',#5708,1.25000000000039,0.785398163397448);
#213=CONICAL_SURFACE('',#5712,1.25000000000025,0.785398163397448);
#214=CONICAL_SURFACE('',#5716,0.750000000000022,0.785398163397449);
#215=CONICAL_SURFACE('',#5720,0.749999999999996,0.785398163397449);
#216=CONICAL_SURFACE('',#5724,0.750000000000014,0.785398163397448);
#217=CONICAL_SURFACE('',#5728,0.750000000000013,0.78539816339745);
#218=CONICAL_SURFACE('',#5732,1.25000000000098,0.78539816339745);
#219=CONICAL_SURFACE('',#5736,99.75,0.785398163397446);
#220=CONICAL_SURFACE('',#5739,5.8095085413358,0.785398163397449);
#221=CONICAL_SURFACE('',#5767,3.40761552865316,0.785398163397446);
#222=CONICAL_SURFACE('',#5770,3.40761552865316,0.785398163397448);
#223=CONICAL_SURFACE('',#5773,3.40761552865316,0.785398163397446);
#224=CONICAL_SURFACE('',#5780,0.7,0.785398163397451);
#225=CONICAL_SURFACE('',#5786,0.7,0.785398163397448);
#226=CONICAL_SURFACE('',#5814,2.90761552865316,0.785398163397448);
#227=CONICAL_SURFACE('',#5848,1.5,0.785398163397448);
#228=CONICAL_SURFACE('',#5852,1.5,0.785398163397448);
#229=CONICAL_SURFACE('',#5856,1.5,0.785398163397448);
#230=CONICAL_SURFACE('',#5860,1.5,0.785398163397448);
#231=CONICAL_SURFACE('',#5864,1.5,0.785398163397448);
#232=CONICAL_SURFACE('',#5886,1.5,0.785398163397448);
#233=CONICAL_SURFACE('',#5887,1.5,0.785398163397448);
#234=CONICAL_SURFACE('',#5888,1.5,0.785398163397448);
#235=CONICAL_SURFACE('',#5890,0.75,0.785398163397447);
#236=CONICAL_SURFACE('',#5893,0.750000000000001,0.785398163397446);
#237=CONICAL_SURFACE('',#5896,0.75,0.785398163397448);
#238=CONICAL_SURFACE('',#5899,2.25,0.785398163397446);
#239=CONICAL_SURFACE('',#5901,0.75,0.785398163397448);
#240=CONICAL_SURFACE('',#5904,0.750000000000001,0.785398163397446);
#241=CONICAL_SURFACE('',#5907,0.749999999999999,0.78539816339745);
#242=CONICAL_SURFACE('',#5910,0.750000000000001,0.785398163397447);
#243=CONICAL_SURFACE('',#5912,2.25,0.785398163397446);
#244=CONICAL_SURFACE('',#5915,0.75,0.785398163397448);
#245=CONICAL_SURFACE('',#5918,0.750000000000001,0.785398163397446);
#246=CONICAL_SURFACE('',#5921,0.75,0.785398163397447);
#247=CONICAL_SURFACE('',#5924,0.749999999999999,0.785398163397449);
#248=CONICAL_SURFACE('',#5927,3.75,0.785398163397447);
#249=CONICAL_SURFACE('',#5930,0.75,0.785398163397448);
#250=CONICAL_SURFACE('',#5954,0.75,0.785398163397447);
#251=CONICAL_SURFACE('',#5956,0.750000000000001,0.785398163397446);
#252=CONICAL_SURFACE('',#5958,0.75,0.785398163397448);
#253=CONICAL_SURFACE('',#5960,2.25,0.785398163397446);
#254=CONICAL_SURFACE('',#5961,0.75,0.785398163397448);
#255=CONICAL_SURFACE('',#5963,0.750000000000001,0.785398163397446);
#256=CONICAL_SURFACE('',#5965,0.749999999999999,0.78539816339745);
#257=CONICAL_SURFACE('',#5967,0.750000000000001,0.785398163397447);
#258=CONICAL_SURFACE('',#5969,2.25,0.785398163397446);
#259=CONICAL_SURFACE('',#5972,0.75,0.785398163397448);
#260=CONICAL_SURFACE('',#5975,0.750000000000001,0.785398163397446);
#261=CONICAL_SURFACE('',#5978,0.75,0.785398163397447);
#262=CONICAL_SURFACE('',#5981,0.749999999999999,0.785398163397449);
#263=CONICAL_SURFACE('',#5984,3.75,0.785398163397447);
#264=CONICAL_SURFACE('',#5987,0.75,0.785398163397448);
#265=CONICAL_SURFACE('',#6005,0.7,0.785398163397451);
#266=CONICAL_SURFACE('',#6011,0.7,0.785398163397448);
#267=CONICAL_SURFACE('',#6032,2.90761552865316,0.785398163397448);
#268=CONICAL_SURFACE('',#6050,0.7,0.785398163397451);
#269=CONICAL_SURFACE('',#6056,0.7,0.785398163397448);
#270=CONICAL_SURFACE('',#6067,0.7,0.785398163397451);
#271=CONICAL_SURFACE('',#6073,0.7,0.785398163397448);
#272=CONICAL_SURFACE('',#6094,2.90761552865316,0.785398163397448);
#273=CIRCLE('',#5503,1.97957176368631);
#274=CIRCLE('',#5504,1.97957176368631);
#275=CIRCLE('',#5507,1.45);
#276=CIRCLE('',#5508,1.45);
#277=CIRCLE('',#5511,1.97957176368631);
#278=CIRCLE('',#5512,1.97957176368631);
#279=CIRCLE('',#5515,1.45);
#280=CIRCLE('',#5516,1.45);
#281=CIRCLE('',#5519,1.97957176368631);
#282=CIRCLE('',#5520,1.97957176368631);
#283=CIRCLE('',#5523,1.45);
#284=CIRCLE('',#5524,1.45);
#285=CIRCLE('',#5527,1.97957176368631);
#286=CIRCLE('',#5528,1.97957176368631);
#287=CIRCLE('',#5531,1.45);
#288=CIRCLE('',#5532,1.45);
#289=CIRCLE('',#5535,1.45);
#290=CIRCLE('',#5536,1.45);
#291=CIRCLE('',#5539,1.97957176368631);
#292=CIRCLE('',#5540,1.97957176368631);
#293=CIRCLE('',#5543,1.45);
#294=CIRCLE('',#5544,1.45);
#295=CIRCLE('',#5547,1.97957176368631);
#296=CIRCLE('',#5548,1.97957176368631);
#297=CIRCLE('',#5551,1.97957176368631);
#298=CIRCLE('',#5552,1.97957176368631);
#299=CIRCLE('',#5555,1.45);
#300=CIRCLE('',#5556,1.45);
#301=CIRCLE('',#5559,1.97957176368631);
#302=CIRCLE('',#5560,1.97957176368631);
#303=CIRCLE('',#5563,1.45);
#304=CIRCLE('',#5564,1.45);
#305=CIRCLE('',#5566,1.77957176368631);
#306=CIRCLE('',#5567,1.77957176368631);
#307=CIRCLE('',#5569,1.77957176368631);
#308=CIRCLE('',#5570,1.77957176368631);
#309=CIRCLE('',#5572,6.0595085413358);
#310=CIRCLE('',#5573,5.5595085413358);
#311=CIRCLE('',#5575,100.);
#312=CIRCLE('',#5576,99.5);
#313=CIRCLE('',#5579,1.50000000000098);
#314=CIRCLE('',#5580,1.00000000000098);
#315=CIRCLE('',#5583,1.00000000000001);
#316=CIRCLE('',#5584,0.500000000000012);
#317=CIRCLE('',#5587,1.00000000000001);
#318=CIRCLE('',#5588,0.500000000000014);
#319=CIRCLE('',#5591,0.999999999999996);
#320=CIRCLE('',#5592,0.499999999999995);
#321=CIRCLE('',#5595,1.00000000000002);
#322=CIRCLE('',#5596,0.500000000000022);
#323=CIRCLE('',#5599,1.50000000000025);
#324=CIRCLE('',#5600,1.00000000000025);
#325=CIRCLE('',#5603,1.50000000000039);
#326=CIRCLE('',#5604,1.00000000000039);
#327=CIRCLE('',#5607,3.80072977423739);
#328=CIRCLE('',#5608,4.30072977423739);
#329=CIRCLE('',#5611,1.00000000000039);
#330=CIRCLE('',#5612,1.50000000000039);
#331=CIRCLE('',#5615,1.00000000000025);
#332=CIRCLE('',#5616,1.50000000000025);
#333=CIRCLE('',#5619,0.500000000000022);
#334=CIRCLE('',#5620,1.00000000000002);
#335=CIRCLE('',#5623,0.499999999999995);
#336=CIRCLE('',#5624,0.999999999999996);
#337=CIRCLE('',#5627,0.500000000000014);
#338=CIRCLE('',#5628,1.00000000000001);
#339=CIRCLE('',#5631,0.500000000000012);
#340=CIRCLE('',#5632,1.00000000000001);
#341=CIRCLE('',#5635,1.00000000000098);
#342=CIRCLE('',#5636,1.50000000000098);
#343=CIRCLE('',#5639,100.);
#344=CIRCLE('',#5640,99.5);
#345=CIRCLE('',#5642,5.5595085413358);
#346=CIRCLE('',#5643,6.0595085413358);
#347=CIRCLE('',#5646,1.50000000000039);
#348=CIRCLE('',#5649,1.50000000000025);
#349=CIRCLE('',#5652,1.00000000000002);
#350=CIRCLE('',#5655,0.999999999999996);
#351=CIRCLE('',#5658,1.00000000000001);
#352=CIRCLE('',#5661,1.00000000000001);
#353=CIRCLE('',#5664,1.50000000000098);
#354=CIRCLE('',#5667,100.);
#355=CIRCLE('',#5669,5.5595085413358);
#356=CIRCLE('',#5671,5.5595085413358);
#357=CIRCLE('',#5673,3.65761552865316);
#358=CIRCLE('',#5674,3.65761552865316);
#359=CIRCLE('',#5675,1.77957176368631);
#360=CIRCLE('',#5676,1.77957176368631);
#361=CIRCLE('',#5677,3.65761552865316);
#362=CIRCLE('',#5679,6.0595085413358);
#363=CIRCLE('',#5681,99.5);
#364=CIRCLE('',#5684,1.00000000000098);
#365=CIRCLE('',#5687,0.500000000000012);
#366=CIRCLE('',#5690,0.500000000000014);
#367=CIRCLE('',#5693,0.499999999999995);
#368=CIRCLE('',#5696,0.500000000000022);
#369=CIRCLE('',#5699,1.00000000000025);
#370=CIRCLE('',#5702,1.00000000000039);
#371=CIRCLE('',#5705,4.30072977423739);
#372=CIRCLE('',#5706,3.80072977423739);
#373=CIRCLE('',#5709,1.00000000000039);
#374=CIRCLE('',#5710,1.50000000000039);
#375=CIRCLE('',#5713,1.00000000000025);
#376=CIRCLE('',#5714,1.50000000000025);
#377=CIRCLE('',#5717,0.500000000000022);
#378=CIRCLE('',#5718,1.00000000000002);
#379=CIRCLE('',#5721,0.499999999999995);
#380=CIRCLE('',#5722,0.999999999999996);
#381=CIRCLE('',#5725,0.500000000000014);
#382=CIRCLE('',#5726,1.00000000000001);
#383=CIRCLE('',#5729,0.500000000000012);
#384=CIRCLE('',#5730,1.00000000000001);
#385=CIRCLE('',#5733,1.00000000000098);
#386=CIRCLE('',#5734,1.50000000000098);
#387=CIRCLE('',#5737,100.);
#388=CIRCLE('',#5738,99.5);
#389=CIRCLE('',#5740,6.0595085413358);
#390=CIRCLE('',#5758,3.15761552865316);
#391=CIRCLE('',#5759,3.15761552865316);
#392=CIRCLE('',#5760,3.15761552865316);
#393=CIRCLE('',#5762,1.77957176368631);
#394=CIRCLE('',#5766,1.77957176368631);
#395=CIRCLE('',#5768,3.15761552865316);
#396=CIRCLE('',#5771,3.15761552865316);
#397=CIRCLE('',#5774,3.15761552865316);
#398=CIRCLE('',#5781,0.649999999999999);
#399=CIRCLE('',#5782,0.75);
#400=CIRCLE('',#5784,0.75);
#401=CIRCLE('',#5787,0.649999999999999);
#402=CIRCLE('',#5791,0.25);
#403=CIRCLE('',#5792,0.75);
#404=CIRCLE('',#5793,0.25);
#405=CIRCLE('',#5794,0.25);
#406=CIRCLE('',#5798,2.59807621135332);
#407=CIRCLE('',#5799,3.);
#408=CIRCLE('',#5801,2.65761552865316);
#409=CIRCLE('',#5802,0.5);
#410=CIRCLE('',#5803,3.15761552865316);
#411=CIRCLE('',#5805,3.15761552865316);
#412=CIRCLE('',#5815,2.65761552865316);
#413=CIRCLE('',#5819,2.59807621135332);
#414=CIRCLE('',#5820,3.);
#415=CIRCLE('',#5822,0.5);
#416=CIRCLE('',#5823,3.5);
#417=CIRCLE('',#5824,0.499999999999998);
#418=CIRCLE('',#5825,0.500000000000001);
#419=CIRCLE('',#5826,0.500000000000002);
#420=CIRCLE('',#5827,0.5);
#421=CIRCLE('',#5828,2.5);
#422=CIRCLE('',#5829,0.500000000000001);
#423=CIRCLE('',#5830,0.499999999999998);
#424=CIRCLE('',#5831,0.500000000000002);
#425=CIRCLE('',#5832,0.5);
#426=CIRCLE('',#5833,2.5);
#427=CIRCLE('',#5834,0.5);
#428=CIRCLE('',#5835,0.500000000000002);
#429=CIRCLE('',#5836,0.500000000000001);
#430=CIRCLE('',#5837,1.75);
#431=CIRCLE('',#5838,1.75);
#432=CIRCLE('',#5839,6.);
#433=CIRCLE('',#5840,1.75);
#434=CIRCLE('',#5841,1.75);
#435=CIRCLE('',#5842,2.59807621135332);
#436=CIRCLE('',#5843,2.59807621135332);
#437=CIRCLE('',#5845,3.);
#438=CIRCLE('',#5847,3.);
#439=CIRCLE('',#5849,1.25);
#440=CIRCLE('',#5851,1.25);
#441=CIRCLE('',#5853,1.25);
#442=CIRCLE('',#5855,1.25);
#443=CIRCLE('',#5857,1.25);
#444=CIRCLE('',#5859,1.25);
#445=CIRCLE('',#5861,1.25);
#446=CIRCLE('',#5863,1.25);
#447=CIRCLE('',#5865,1.75);
#448=CIRCLE('',#5867,0.500000000000001);
#449=CIRCLE('',#5868,0.500000000000002);
#450=CIRCLE('',#5869,0.5);
#451=CIRCLE('',#5870,2.5);
#452=CIRCLE('',#5871,0.5);
#453=CIRCLE('',#5872,0.500000000000002);
#454=CIRCLE('',#5873,0.499999999999998);
#455=CIRCLE('',#5874,0.500000000000001);
#456=CIRCLE('',#5875,2.5);
#457=CIRCLE('',#5876,0.5);
#458=CIRCLE('',#5877,0.500000000000002);
#459=CIRCLE('',#5878,0.500000000000001);
#460=CIRCLE('',#5879,0.499999999999998);
#461=CIRCLE('',#5880,3.5);
#462=CIRCLE('',#5881,0.5);
#463=CIRCLE('',#5882,1.75);
#464=CIRCLE('',#5883,1.75);
#465=CIRCLE('',#5884,6.);
#466=CIRCLE('',#5885,1.75);
#467=CIRCLE('',#5891,1.);
#468=CIRCLE('',#5894,1.);
#469=CIRCLE('',#5897,1.);
#470=CIRCLE('',#5900,2.);
#471=CIRCLE('',#5902,1.);
#472=CIRCLE('',#5905,1.);
#473=CIRCLE('',#5908,1.);
#474=CIRCLE('',#5911,1.);
#475=CIRCLE('',#5913,2.);
#476=CIRCLE('',#5916,1.);
#477=CIRCLE('',#5919,1.);
#478=CIRCLE('',#5922,1.);
#479=CIRCLE('',#5925,1.);
#480=CIRCLE('',#5928,4.);
#481=CIRCLE('',#5931,1.);
#482=CIRCLE('',#5934,1.);
#483=CIRCLE('',#5937,1.);
#484=CIRCLE('',#5940,1.);
#485=CIRCLE('',#5942,2.);
#486=CIRCLE('',#5945,1.);
#487=CIRCLE('',#5948,1.);
#488=CIRCLE('',#5951,1.);
#489=CIRCLE('',#5968,1.);
#490=CIRCLE('',#5970,2.);
#491=CIRCLE('',#5973,1.);
#492=CIRCLE('',#5976,1.);
#493=CIRCLE('',#5979,1.);
#494=CIRCLE('',#5982,1.);
#495=CIRCLE('',#5985,4.);
#496=CIRCLE('',#5988,1.);
#497=CIRCLE('',#6006,0.649999999999999);
#498=CIRCLE('',#6007,0.75);
#499=CIRCLE('',#6009,0.75);
#500=CIRCLE('',#6012,0.649999999999999);
#501=CIRCLE('',#6016,2.59807621135332);
#502=CIRCLE('',#6017,3.);
#503=CIRCLE('',#6019,2.65761552865316);
#504=CIRCLE('',#6020,0.5);
#505=CIRCLE('',#6021,3.15761552865316);
#506=CIRCLE('',#6023,3.15761552865316);
#507=CIRCLE('',#6033,2.65761552865316);
#508=CIRCLE('',#6037,0.25);
#509=CIRCLE('',#6038,0.75);
#510=CIRCLE('',#6039,0.25);
#511=CIRCLE('',#6040,0.25);
#512=CIRCLE('',#6044,0.25);
#513=CIRCLE('',#6045,0.75);
#514=CIRCLE('',#6046,0.25);
#515=CIRCLE('',#6047,0.25);
#516=CIRCLE('',#6051,0.649999999999999);
#517=CIRCLE('',#6052,0.75);
#518=CIRCLE('',#6054,0.75);
#519=CIRCLE('',#6057,0.649999999999999);
#520=CIRCLE('',#6061,0.25);
#521=CIRCLE('',#6062,0.75);
#522=CIRCLE('',#6063,0.25);
#523=CIRCLE('',#6064,0.25);
#524=CIRCLE('',#6068,0.649999999999999);
#525=CIRCLE('',#6069,0.75);
#526=CIRCLE('',#6071,0.75);
#527=CIRCLE('',#6074,0.649999999999999);
#528=CIRCLE('',#6078,2.59807621135332);
#529=CIRCLE('',#6079,3.);
#530=CIRCLE('',#6081,2.65761552865316);
#531=CIRCLE('',#6082,0.5);
#532=CIRCLE('',#6083,3.15761552865316);
#533=CIRCLE('',#6085,3.15761552865316);
#534=CIRCLE('',#6095,2.65761552865316);
#535=CYLINDRICAL_SURFACE('',#5502,1.97957176368631);
#536=CYLINDRICAL_SURFACE('',#5506,1.45);
#537=CYLINDRICAL_SURFACE('',#5510,1.97957176368631);
#538=CYLINDRICAL_SURFACE('',#5514,1.45);
#539=CYLINDRICAL_SURFACE('',#5518,1.97957176368631);
#540=CYLINDRICAL_SURFACE('',#5522,1.45);
#541=CYLINDRICAL_SURFACE('',#5526,1.97957176368631);
#542=CYLINDRICAL_SURFACE('',#5530,1.45);
#543=CYLINDRICAL_SURFACE('',#5534,1.45);
#544=CYLINDRICAL_SURFACE('',#5538,1.97957176368631);
#545=CYLINDRICAL_SURFACE('',#5542,1.45);
#546=CYLINDRICAL_SURFACE('',#5546,1.97957176368631);
#547=CYLINDRICAL_SURFACE('',#5550,1.97957176368631);
#548=CYLINDRICAL_SURFACE('',#5554,1.45);
#549=CYLINDRICAL_SURFACE('',#5558,1.97957176368631);
#550=CYLINDRICAL_SURFACE('',#5562,1.45);
#551=CYLINDRICAL_SURFACE('',#5565,1.77957176368631);
#552=CYLINDRICAL_SURFACE('',#5568,1.77957176368631);
#553=CYLINDRICAL_SURFACE('',#5645,1.50000000000039);
#554=CYLINDRICAL_SURFACE('',#5648,1.50000000000025);
#555=CYLINDRICAL_SURFACE('',#5651,1.00000000000002);
#556=CYLINDRICAL_SURFACE('',#5654,0.999999999999996);
#557=CYLINDRICAL_SURFACE('',#5657,1.00000000000001);
#558=CYLINDRICAL_SURFACE('',#5660,1.00000000000001);
#559=CYLINDRICAL_SURFACE('',#5663,1.50000000000098);
#560=CYLINDRICAL_SURFACE('',#5666,100.);
#561=CYLINDRICAL_SURFACE('',#5668,5.5595085413358);
#562=CYLINDRICAL_SURFACE('',#5670,5.5595085413358);
#563=CYLINDRICAL_SURFACE('',#5742,1.50000000000039);
#564=CYLINDRICAL_SURFACE('',#5744,1.50000000000025);
#565=CYLINDRICAL_SURFACE('',#5746,1.00000000000002);
#566=CYLINDRICAL_SURFACE('',#5748,0.999999999999996);
#567=CYLINDRICAL_SURFACE('',#5750,1.00000000000001);
#568=CYLINDRICAL_SURFACE('',#5752,1.00000000000001);
#569=CYLINDRICAL_SURFACE('',#5754,1.50000000000098);
#570=CYLINDRICAL_SURFACE('',#5756,100.);
#571=CYLINDRICAL_SURFACE('',#5769,3.15761552865316);
#572=CYLINDRICAL_SURFACE('',#5772,3.15761552865316);
#573=CYLINDRICAL_SURFACE('',#5775,3.15761552865316);
#574=CYLINDRICAL_SURFACE('',#5776,1.77957176368631);
#575=CYLINDRICAL_SURFACE('',#5777,1.77957176368631);
#576=CYLINDRICAL_SURFACE('',#5778,4.30072977423739);
#577=CYLINDRICAL_SURFACE('',#5783,0.75);
#578=CYLINDRICAL_SURFACE('',#5804,3.15761552865316);
#579=CYLINDRICAL_SURFACE('',#5850,1.25);
#580=CYLINDRICAL_SURFACE('',#5854,1.25);
#581=CYLINDRICAL_SURFACE('',#5858,1.25);
#582=CYLINDRICAL_SURFACE('',#5862,1.25);
#583=CYLINDRICAL_SURFACE('',#5933,1.);
#584=CYLINDRICAL_SURFACE('',#5936,1.);
#585=CYLINDRICAL_SURFACE('',#5939,1.);
#586=CYLINDRICAL_SURFACE('',#5941,2.);
#587=CYLINDRICAL_SURFACE('',#5944,1.);
#588=CYLINDRICAL_SURFACE('',#5947,1.);
#589=CYLINDRICAL_SURFACE('',#5950,1.);
#590=CYLINDRICAL_SURFACE('',#5989,2.);
#591=CYLINDRICAL_SURFACE('',#5991,1.);
#592=CYLINDRICAL_SURFACE('',#5993,1.);
#593=CYLINDRICAL_SURFACE('',#5995,1.);
#594=CYLINDRICAL_SURFACE('',#5997,1.);
#595=CYLINDRICAL_SURFACE('',#5999,4.);
#596=CYLINDRICAL_SURFACE('',#6001,1.);
#597=CYLINDRICAL_SURFACE('',#6002,1.);
#598=CYLINDRICAL_SURFACE('',#6003,6.);
#599=CYLINDRICAL_SURFACE('',#6008,0.75);
#600=CYLINDRICAL_SURFACE('',#6022,3.15761552865316);
#601=CYLINDRICAL_SURFACE('',#6053,0.75);
#602=CYLINDRICAL_SURFACE('',#6070,0.75);
#603=CYLINDRICAL_SURFACE('',#6084,3.15761552865316);
#604=FACE_OUTER_BOUND('',#930,.T.);
#605=FACE_OUTER_BOUND('',#931,.T.);
#606=FACE_OUTER_BOUND('',#932,.T.);
#607=FACE_OUTER_BOUND('',#933,.T.);
#608=FACE_OUTER_BOUND('',#934,.T.);
#609=FACE_OUTER_BOUND('',#935,.T.);
#610=FACE_OUTER_BOUND('',#936,.T.);
#611=FACE_OUTER_BOUND('',#937,.T.);
#612=FACE_OUTER_BOUND('',#938,.T.);
#613=FACE_OUTER_BOUND('',#939,.T.);
#614=FACE_OUTER_BOUND('',#940,.T.);
#615=FACE_OUTER_BOUND('',#941,.T.);
#616=FACE_OUTER_BOUND('',#942,.T.);
#617=FACE_OUTER_BOUND('',#943,.T.);
#618=FACE_OUTER_BOUND('',#944,.T.);
#619=FACE_OUTER_BOUND('',#945,.T.);
#620=FACE_OUTER_BOUND('',#946,.T.);
#621=FACE_OUTER_BOUND('',#947,.T.);
#622=FACE_OUTER_BOUND('',#948,.T.);
#623=FACE_OUTER_BOUND('',#949,.T.);
#624=FACE_OUTER_BOUND('',#950,.T.);
#625=FACE_OUTER_BOUND('',#951,.T.);
#626=FACE_OUTER_BOUND('',#952,.T.);
#627=FACE_OUTER_BOUND('',#953,.T.);
#628=FACE_OUTER_BOUND('',#954,.T.);
#629=FACE_OUTER_BOUND('',#955,.T.);
#630=FACE_OUTER_BOUND('',#956,.T.);
#631=FACE_OUTER_BOUND('',#957,.T.);
#632=FACE_OUTER_BOUND('',#958,.T.);
#633=FACE_OUTER_BOUND('',#959,.T.);
#634=FACE_OUTER_BOUND('',#960,.T.);
#635=FACE_OUTER_BOUND('',#961,.T.);
#636=FACE_OUTER_BOUND('',#962,.T.);
#637=FACE_OUTER_BOUND('',#963,.T.);
#638=FACE_OUTER_BOUND('',#964,.T.);
#639=FACE_OUTER_BOUND('',#965,.T.);
#640=FACE_OUTER_BOUND('',#966,.T.);
#641=FACE_OUTER_BOUND('',#967,.T.);
#642=FACE_OUTER_BOUND('',#968,.T.);
#643=FACE_OUTER_BOUND('',#969,.T.);
#644=FACE_OUTER_BOUND('',#970,.T.);
#645=FACE_OUTER_BOUND('',#971,.T.);
#646=FACE_OUTER_BOUND('',#972,.T.);
#647=FACE_OUTER_BOUND('',#973,.T.);
#648=FACE_OUTER_BOUND('',#974,.T.);
#649=FACE_OUTER_BOUND('',#975,.T.);
#650=FACE_OUTER_BOUND('',#976,.T.);
#651=FACE_OUTER_BOUND('',#977,.T.);
#652=FACE_OUTER_BOUND('',#978,.T.);
#653=FACE_OUTER_BOUND('',#979,.T.);
#654=FACE_OUTER_BOUND('',#980,.T.);
#655=FACE_OUTER_BOUND('',#981,.T.);
#656=FACE_OUTER_BOUND('',#982,.T.);
#657=FACE_OUTER_BOUND('',#983,.T.);
#658=FACE_OUTER_BOUND('',#984,.T.);
#659=FACE_OUTER_BOUND('',#985,.T.);
#660=FACE_OUTER_BOUND('',#986,.T.);
#661=FACE_OUTER_BOUND('',#987,.T.);
#662=FACE_OUTER_BOUND('',#988,.T.);
#663=FACE_OUTER_BOUND('',#989,.T.);
#664=FACE_OUTER_BOUND('',#990,.T.);
#665=FACE_OUTER_BOUND('',#991,.T.);
#666=FACE_OUTER_BOUND('',#992,.T.);
#667=FACE_OUTER_BOUND('',#993,.T.);
#668=FACE_OUTER_BOUND('',#994,.T.);
#669=FACE_OUTER_BOUND('',#995,.T.);
#670=FACE_OUTER_BOUND('',#996,.T.);
#671=FACE_OUTER_BOUND('',#997,.T.);
#672=FACE_OUTER_BOUND('',#998,.T.);
#673=FACE_OUTER_BOUND('',#999,.T.);
#674=FACE_OUTER_BOUND('',#1000,.T.);
#675=FACE_OUTER_BOUND('',#1001,.T.);
#676=FACE_OUTER_BOUND('',#1002,.T.);
#677=FACE_OUTER_BOUND('',#1003,.T.);
#678=FACE_OUTER_BOUND('',#1004,.T.);
#679=FACE_OUTER_BOUND('',#1005,.T.);
#680=FACE_OUTER_BOUND('',#1006,.T.);
#681=FACE_OUTER_BOUND('',#1007,.T.);
#682=FACE_OUTER_BOUND('',#1008,.T.);
#683=FACE_OUTER_BOUND('',#1009,.T.);
#684=FACE_OUTER_BOUND('',#1010,.T.);
#685=FACE_OUTER_BOUND('',#1011,.T.);
#686=FACE_OUTER_BOUND('',#1012,.T.);
#687=FACE_OUTER_BOUND('',#1013,.T.);
#688=FACE_OUTER_BOUND('',#1014,.T.);
#689=FACE_OUTER_BOUND('',#1015,.T.);
#690=FACE_OUTER_BOUND('',#1016,.T.);
#691=FACE_OUTER_BOUND('',#1017,.T.);
#692=FACE_OUTER_BOUND('',#1025,.T.);
#693=FACE_OUTER_BOUND('',#1026,.T.);
#694=FACE_OUTER_BOUND('',#1027,.T.);
#695=FACE_OUTER_BOUND('',#1028,.T.);
#696=FACE_OUTER_BOUND('',#1029,.T.);
#697=FACE_OUTER_BOUND('',#1030,.T.);
#698=FACE_OUTER_BOUND('',#1031,.T.);
#699=FACE_OUTER_BOUND('',#1032,.T.);
#700=FACE_OUTER_BOUND('',#1033,.T.);
#701=FACE_OUTER_BOUND('',#1034,.T.);
#702=FACE_OUTER_BOUND('',#1035,.T.);
#703=FACE_OUTER_BOUND('',#1036,.T.);
#704=FACE_OUTER_BOUND('',#1037,.T.);
#705=FACE_OUTER_BOUND('',#1038,.T.);
#706=FACE_OUTER_BOUND('',#1039,.T.);
#707=FACE_OUTER_BOUND('',#1040,.T.);
#708=FACE_OUTER_BOUND('',#1041,.T.);
#709=FACE_OUTER_BOUND('',#1042,.T.);
#710=FACE_OUTER_BOUND('',#1043,.T.);
#711=FACE_OUTER_BOUND('',#1044,.T.);
#712=FACE_OUTER_BOUND('',#1045,.T.);
#713=FACE_OUTER_BOUND('',#1046,.T.);
#714=FACE_OUTER_BOUND('',#1047,.T.);
#715=FACE_OUTER_BOUND('',#1048,.T.);
#716=FACE_OUTER_BOUND('',#1049,.T.);
#717=FACE_OUTER_BOUND('',#1050,.T.);
#718=FACE_OUTER_BOUND('',#1051,.T.);
#719=FACE_OUTER_BOUND('',#1052,.T.);
#720=FACE_OUTER_BOUND('',#1053,.T.);
#721=FACE_OUTER_BOUND('',#1054,.T.);
#722=FACE_OUTER_BOUND('',#1055,.T.);
#723=FACE_OUTER_BOUND('',#1056,.T.);
#724=FACE_OUTER_BOUND('',#1057,.T.);
#725=FACE_OUTER_BOUND('',#1058,.T.);
#726=FACE_OUTER_BOUND('',#1059,.T.);
#727=FACE_OUTER_BOUND('',#1060,.T.);
#728=FACE_OUTER_BOUND('',#1061,.T.);
#729=FACE_OUTER_BOUND('',#1062,.T.);
#730=FACE_OUTER_BOUND('',#1063,.T.);
#731=FACE_OUTER_BOUND('',#1064,.T.);
#732=FACE_OUTER_BOUND('',#1065,.T.);
#733=FACE_OUTER_BOUND('',#1066,.T.);
#734=FACE_OUTER_BOUND('',#1067,.T.);
#735=FACE_OUTER_BOUND('',#1068,.T.);
#736=FACE_OUTER_BOUND('',#1069,.T.);
#737=FACE_OUTER_BOUND('',#1070,.T.);
#738=FACE_OUTER_BOUND('',#1071,.T.);
#739=FACE_OUTER_BOUND('',#1072,.T.);
#740=FACE_OUTER_BOUND('',#1073,.T.);
#741=FACE_OUTER_BOUND('',#1074,.T.);
#742=FACE_OUTER_BOUND('',#1075,.T.);
#743=FACE_OUTER_BOUND('',#1076,.T.);
#744=FACE_OUTER_BOUND('',#1084,.T.);
#745=FACE_OUTER_BOUND('',#1086,.T.);
#746=FACE_OUTER_BOUND('',#1088,.T.);
#747=FACE_OUTER_BOUND('',#1090,.T.);
#748=FACE_OUTER_BOUND('',#1092,.T.);
#749=FACE_OUTER_BOUND('',#1093,.T.);
#750=FACE_OUTER_BOUND('',#1094,.T.);
#751=FACE_OUTER_BOUND('',#1095,.T.);
#752=FACE_OUTER_BOUND('',#1096,.T.);
#753=FACE_OUTER_BOUND('',#1097,.T.);
#754=FACE_OUTER_BOUND('',#1098,.T.);
#755=FACE_OUTER_BOUND('',#1099,.T.);
#756=FACE_OUTER_BOUND('',#1100,.T.);
#757=FACE_OUTER_BOUND('',#1101,.T.);
#758=FACE_OUTER_BOUND('',#1102,.T.);
#759=FACE_OUTER_BOUND('',#1103,.T.);
#760=FACE_OUTER_BOUND('',#1104,.T.);
#761=FACE_OUTER_BOUND('',#1105,.T.);
#762=FACE_OUTER_BOUND('',#1106,.T.);
#763=FACE_OUTER_BOUND('',#1108,.T.);
#764=FACE_OUTER_BOUND('',#1109,.T.);
#765=FACE_OUTER_BOUND('',#1110,.T.);
#766=FACE_OUTER_BOUND('',#1111,.T.);
#767=FACE_OUTER_BOUND('',#1112,.T.);
#768=FACE_OUTER_BOUND('',#1113,.T.);
#769=FACE_OUTER_BOUND('',#1115,.T.);
#770=FACE_OUTER_BOUND('',#1116,.T.);
#771=FACE_OUTER_BOUND('',#1117,.T.);
#772=FACE_OUTER_BOUND('',#1118,.T.);
#773=FACE_OUTER_BOUND('',#1119,.T.);
#774=FACE_OUTER_BOUND('',#1120,.T.);
#775=FACE_OUTER_BOUND('',#1121,.T.);
#776=FACE_OUTER_BOUND('',#1122,.T.);
#777=FACE_OUTER_BOUND('',#1123,.T.);
#778=FACE_OUTER_BOUND('',#1125,.T.);
#779=FACE_OUTER_BOUND('',#1126,.T.);
#780=FACE_OUTER_BOUND('',#1135,.T.);
#781=FACE_OUTER_BOUND('',#1136,.T.);
#782=FACE_OUTER_BOUND('',#1137,.T.);
#783=FACE_OUTER_BOUND('',#1138,.T.);
#784=FACE_OUTER_BOUND('',#1139,.T.);
#785=FACE_OUTER_BOUND('',#1140,.T.);
#786=FACE_OUTER_BOUND('',#1141,.T.);
#787=FACE_OUTER_BOUND('',#1142,.T.);
#788=FACE_OUTER_BOUND('',#1143,.T.);
#789=FACE_OUTER_BOUND('',#1144,.T.);
#790=FACE_OUTER_BOUND('',#1145,.T.);
#791=FACE_OUTER_BOUND('',#1146,.T.);
#792=FACE_OUTER_BOUND('',#1152,.T.);
#793=FACE_OUTER_BOUND('',#1153,.T.);
#794=FACE_OUTER_BOUND('',#1154,.T.);
#795=FACE_OUTER_BOUND('',#1155,.T.);
#796=FACE_OUTER_BOUND('',#1156,.T.);
#797=FACE_OUTER_BOUND('',#1157,.T.);
#798=FACE_OUTER_BOUND('',#1158,.T.);
#799=FACE_OUTER_BOUND('',#1159,.T.);
#800=FACE_OUTER_BOUND('',#1160,.T.);
#801=FACE_OUTER_BOUND('',#1161,.T.);
#802=FACE_OUTER_BOUND('',#1162,.T.);
#803=FACE_OUTER_BOUND('',#1163,.T.);
#804=FACE_OUTER_BOUND('',#1164,.T.);
#805=FACE_OUTER_BOUND('',#1165,.T.);
#806=FACE_OUTER_BOUND('',#1166,.T.);
#807=FACE_OUTER_BOUND('',#1167,.T.);
#808=FACE_OUTER_BOUND('',#1168,.T.);
#809=FACE_OUTER_BOUND('',#1169,.T.);
#810=FACE_OUTER_BOUND('',#1170,.T.);
#811=FACE_OUTER_BOUND('',#1171,.T.);
#812=FACE_OUTER_BOUND('',#1172,.T.);
#813=FACE_OUTER_BOUND('',#1173,.T.);
#814=FACE_OUTER_BOUND('',#1174,.T.);
#815=FACE_OUTER_BOUND('',#1175,.T.);
#816=FACE_OUTER_BOUND('',#1176,.T.);
#817=FACE_OUTER_BOUND('',#1177,.T.);
#818=FACE_OUTER_BOUND('',#1178,.T.);
#819=FACE_OUTER_BOUND('',#1179,.T.);
#820=FACE_OUTER_BOUND('',#1180,.T.);
#821=FACE_OUTER_BOUND('',#1181,.T.);
#822=FACE_OUTER_BOUND('',#1182,.T.);
#823=FACE_OUTER_BOUND('',#1183,.T.);
#824=FACE_OUTER_BOUND('',#1184,.T.);
#825=FACE_OUTER_BOUND('',#1185,.T.);
#826=FACE_OUTER_BOUND('',#1186,.T.);
#827=FACE_OUTER_BOUND('',#1187,.T.);
#828=FACE_OUTER_BOUND('',#1188,.T.);
#829=FACE_OUTER_BOUND('',#1189,.T.);
#830=FACE_OUTER_BOUND('',#1190,.T.);
#831=FACE_OUTER_BOUND('',#1191,.T.);
#832=FACE_OUTER_BOUND('',#1192,.T.);
#833=FACE_OUTER_BOUND('',#1193,.T.);
#834=FACE_OUTER_BOUND('',#1194,.T.);
#835=FACE_OUTER_BOUND('',#1195,.T.);
#836=FACE_OUTER_BOUND('',#1196,.T.);
#837=FACE_OUTER_BOUND('',#1197,.T.);
#838=FACE_OUTER_BOUND('',#1198,.T.);
#839=FACE_OUTER_BOUND('',#1199,.T.);
#840=FACE_OUTER_BOUND('',#1200,.T.);
#841=FACE_OUTER_BOUND('',#1201,.T.);
#842=FACE_OUTER_BOUND('',#1202,.T.);
#843=FACE_OUTER_BOUND('',#1203,.T.);
#844=FACE_OUTER_BOUND('',#1204,.T.);
#845=FACE_OUTER_BOUND('',#1205,.T.);
#846=FACE_OUTER_BOUND('',#1206,.T.);
#847=FACE_OUTER_BOUND('',#1207,.T.);
#848=FACE_OUTER_BOUND('',#1208,.T.);
#849=FACE_OUTER_BOUND('',#1209,.T.);
#850=FACE_OUTER_BOUND('',#1210,.T.);
#851=FACE_OUTER_BOUND('',#1211,.T.);
#852=FACE_OUTER_BOUND('',#1212,.T.);
#853=FACE_OUTER_BOUND('',#1213,.T.);
#854=FACE_OUTER_BOUND('',#1214,.T.);
#855=FACE_OUTER_BOUND('',#1215,.T.);
#856=FACE_OUTER_BOUND('',#1216,.T.);
#857=FACE_OUTER_BOUND('',#1217,.T.);
#858=FACE_OUTER_BOUND('',#1218,.T.);
#859=FACE_OUTER_BOUND('',#1219,.T.);
#860=FACE_OUTER_BOUND('',#1220,.T.);
#861=FACE_OUTER_BOUND('',#1221,.T.);
#862=FACE_OUTER_BOUND('',#1222,.T.);
#863=FACE_OUTER_BOUND('',#1223,.T.);
#864=FACE_OUTER_BOUND('',#1224,.T.);
#865=FACE_OUTER_BOUND('',#1225,.T.);
#866=FACE_OUTER_BOUND('',#1226,.T.);
#867=FACE_OUTER_BOUND('',#1227,.T.);
#868=FACE_OUTER_BOUND('',#1228,.T.);
#869=FACE_OUTER_BOUND('',#1229,.T.);
#870=FACE_OUTER_BOUND('',#1230,.T.);
#871=FACE_OUTER_BOUND('',#1231,.T.);
#872=FACE_OUTER_BOUND('',#1232,.T.);
#873=FACE_OUTER_BOUND('',#1233,.T.);
#874=FACE_OUTER_BOUND('',#1234,.T.);
#875=FACE_OUTER_BOUND('',#1235,.T.);
#876=FACE_OUTER_BOUND('',#1236,.T.);
#877=FACE_OUTER_BOUND('',#1237,.T.);
#878=FACE_OUTER_BOUND('',#1238,.T.);
#879=FACE_OUTER_BOUND('',#1239,.T.);
#880=FACE_OUTER_BOUND('',#1240,.T.);
#881=FACE_OUTER_BOUND('',#1241,.T.);
#882=FACE_OUTER_BOUND('',#1242,.T.);
#883=FACE_OUTER_BOUND('',#1243,.T.);
#884=FACE_OUTER_BOUND('',#1244,.T.);
#885=FACE_OUTER_BOUND('',#1245,.T.);
#886=FACE_OUTER_BOUND('',#1246,.T.);
#887=FACE_OUTER_BOUND('',#1247,.T.);
#888=FACE_OUTER_BOUND('',#1248,.T.);
#889=FACE_OUTER_BOUND('',#1250,.T.);
#890=FACE_OUTER_BOUND('',#1251,.T.);
#891=FACE_OUTER_BOUND('',#1252,.T.);
#892=FACE_OUTER_BOUND('',#1253,.T.);
#893=FACE_OUTER_BOUND('',#1254,.T.);
#894=FACE_OUTER_BOUND('',#1255,.T.);
#895=FACE_OUTER_BOUND('',#1256,.T.);
#896=FACE_OUTER_BOUND('',#1257,.T.);
#897=FACE_OUTER_BOUND('',#1258,.T.);
#898=FACE_OUTER_BOUND('',#1260,.T.);
#899=FACE_OUTER_BOUND('',#1262,.T.);
#900=FACE_OUTER_BOUND('',#1263,.T.);
#901=FACE_OUTER_BOUND('',#1264,.T.);
#902=FACE_OUTER_BOUND('',#1266,.T.);
#903=FACE_OUTER_BOUND('',#1267,.T.);
#904=FACE_OUTER_BOUND('',#1268,.T.);
#905=FACE_OUTER_BOUND('',#1269,.T.);
#906=FACE_OUTER_BOUND('',#1270,.T.);
#907=FACE_OUTER_BOUND('',#1271,.T.);
#908=FACE_OUTER_BOUND('',#1272,.T.);
#909=FACE_OUTER_BOUND('',#1273,.T.);
#910=FACE_OUTER_BOUND('',#1275,.T.);
#911=FACE_OUTER_BOUND('',#1276,.T.);
#912=FACE_OUTER_BOUND('',#1277,.T.);
#913=FACE_OUTER_BOUND('',#1278,.T.);
#914=FACE_OUTER_BOUND('',#1279,.T.);
#915=FACE_OUTER_BOUND('',#1280,.T.);
#916=FACE_OUTER_BOUND('',#1281,.T.);
#917=FACE_OUTER_BOUND('',#1282,.T.);
#918=FACE_OUTER_BOUND('',#1283,.T.);
#919=FACE_OUTER_BOUND('',#1284,.T.);
#920=FACE_OUTER_BOUND('',#1285,.T.);
#921=FACE_OUTER_BOUND('',#1287,.T.);
#922=FACE_OUTER_BOUND('',#1288,.T.);
#923=FACE_OUTER_BOUND('',#1289,.T.);
#924=FACE_OUTER_BOUND('',#1290,.T.);
#925=FACE_OUTER_BOUND('',#1291,.T.);
#926=FACE_OUTER_BOUND('',#1292,.T.);
#927=FACE_OUTER_BOUND('',#1293,.T.);
#928=FACE_OUTER_BOUND('',#1294,.T.);
#929=FACE_OUTER_BOUND('',#1295,.T.);
#930=EDGE_LOOP('',(#3398,#3399,#3400,#3401));
#931=EDGE_LOOP('',(#3402,#3403,#3404,#3405));
#932=EDGE_LOOP('',(#3406,#3407,#3408,#3409));
#933=EDGE_LOOP('',(#3410,#3411,#3412,#3413));
#934=EDGE_LOOP('',(#3414,#3415,#3416,#3417));
#935=EDGE_LOOP('',(#3418,#3419,#3420,#3421));
#936=EDGE_LOOP('',(#3422,#3423,#3424,#3425));
#937=EDGE_LOOP('',(#3426,#3427,#3428,#3429));
#938=EDGE_LOOP('',(#3430,#3431,#3432,#3433));
#939=EDGE_LOOP('',(#3434,#3435,#3436,#3437));
#940=EDGE_LOOP('',(#3438,#3439,#3440,#3441));
#941=EDGE_LOOP('',(#3442,#3443,#3444,#3445));
#942=EDGE_LOOP('',(#3446,#3447,#3448,#3449));
#943=EDGE_LOOP('',(#3450,#3451,#3452,#3453));
#944=EDGE_LOOP('',(#3454,#3455,#3456,#3457));
#945=EDGE_LOOP('',(#3458,#3459,#3460,#3461));
#946=EDGE_LOOP('',(#3462,#3463,#3464,#3465));
#947=EDGE_LOOP('',(#3466,#3467,#3468,#3469));
#948=EDGE_LOOP('',(#3470,#3471,#3472,#3473));
#949=EDGE_LOOP('',(#3474,#3475,#3476,#3477));
#950=EDGE_LOOP('',(#3478,#3479,#3480,#3481));
#951=EDGE_LOOP('',(#3482,#3483,#3484,#3485));
#952=EDGE_LOOP('',(#3486,#3487,#3488,#3489));
#953=EDGE_LOOP('',(#3490,#3491,#3492,#3493));
#954=EDGE_LOOP('',(#3494,#3495,#3496,#3497));
#955=EDGE_LOOP('',(#3498,#3499,#3500,#3501));
#956=EDGE_LOOP('',(#3502,#3503,#3504,#3505));
#957=EDGE_LOOP('',(#3506,#3507,#3508,#3509));
#958=EDGE_LOOP('',(#3510,#3511,#3512,#3513));
#959=EDGE_LOOP('',(#3514,#3515,#3516,#3517));
#960=EDGE_LOOP('',(#3518,#3519,#3520,#3521));
#961=EDGE_LOOP('',(#3522,#3523,#3524,#3525));
#962=EDGE_LOOP('',(#3526,#3527,#3528,#3529));
#963=EDGE_LOOP('',(#3530,#3531,#3532,#3533));
#964=EDGE_LOOP('',(#3534,#3535,#3536,#3537));
#965=EDGE_LOOP('',(#3538,#3539,#3540,#3541));
#966=EDGE_LOOP('',(#3542,#3543,#3544,#3545));
#967=EDGE_LOOP('',(#3546,#3547,#3548,#3549));
#968=EDGE_LOOP('',(#3550,#3551,#3552,#3553));
#969=EDGE_LOOP('',(#3554,#3555,#3556,#3557));
#970=EDGE_LOOP('',(#3558,#3559,#3560,#3561));
#971=EDGE_LOOP('',(#3562,#3563,#3564,#3565));
#972=EDGE_LOOP('',(#3566,#3567,#3568,#3569));
#973=EDGE_LOOP('',(#3570,#3571,#3572,#3573));
#974=EDGE_LOOP('',(#3574,#3575,#3576,#3577));
#975=EDGE_LOOP('',(#3578,#3579,#3580,#3581));
#976=EDGE_LOOP('',(#3582,#3583,#3584,#3585));
#977=EDGE_LOOP('',(#3586,#3587,#3588,#3589));
#978=EDGE_LOOP('',(#3590,#3591,#3592,#3593));
#979=EDGE_LOOP('',(#3594,#3595,#3596,#3597));
#980=EDGE_LOOP('',(#3598,#3599,#3600,#3601));
#981=EDGE_LOOP('',(#3602,#3603,#3604,#3605));
#982=EDGE_LOOP('',(#3606,#3607,#3608,#3609));
#983=EDGE_LOOP('',(#3610,#3611,#3612,#3613));
#984=EDGE_LOOP('',(#3614,#3615,#3616,#3617));
#985=EDGE_LOOP('',(#3618,#3619,#3620,#3621));
#986=EDGE_LOOP('',(#3622,#3623,#3624,#3625));
#987=EDGE_LOOP('',(#3626,#3627,#3628,#3629));
#988=EDGE_LOOP('',(#3630,#3631,#3632,#3633));
#989=EDGE_LOOP('',(#3634,#3635,#3636,#3637));
#990=EDGE_LOOP('',(#3638,#3639,#3640,#3641));
#991=EDGE_LOOP('',(#3642,#3643,#3644,#3645));
#992=EDGE_LOOP('',(#3646,#3647,#3648,#3649));
#993=EDGE_LOOP('',(#3650,#3651,#3652,#3653));
#994=EDGE_LOOP('',(#3654,#3655,#3656,#3657));
#995=EDGE_LOOP('',(#3658,#3659,#3660,#3661));
#996=EDGE_LOOP('',(#3662,#3663,#3664,#3665));
#997=EDGE_LOOP('',(#3666,#3667,#3668,#3669));
#998=EDGE_LOOP('',(#3670,#3671,#3672,#3673));
#999=EDGE_LOOP('',(#3674,#3675,#3676,#3677));
#1000=EDGE_LOOP('',(#3678,#3679,#3680,#3681));
#1001=EDGE_LOOP('',(#3682,#3683,#3684,#3685));
#1002=EDGE_LOOP('',(#3686,#3687,#3688,#3689));
#1003=EDGE_LOOP('',(#3690,#3691,#3692,#3693));
#1004=EDGE_LOOP('',(#3694,#3695,#3696,#3697));
#1005=EDGE_LOOP('',(#3698,#3699,#3700,#3701));
#1006=EDGE_LOOP('',(#3702,#3703,#3704,#3705));
#1007=EDGE_LOOP('',(#3706,#3707,#3708,#3709));
#1008=EDGE_LOOP('',(#3710,#3711,#3712,#3713));
#1009=EDGE_LOOP('',(#3714,#3715,#3716,#3717));
#1010=EDGE_LOOP('',(#3718,#3719,#3720,#3721));
#1011=EDGE_LOOP('',(#3722,#3723,#3724,#3725));
#1012=EDGE_LOOP('',(#3726,#3727,#3728,#3729));
#1013=EDGE_LOOP('',(#3730,#3731,#3732,#3733));
#1014=EDGE_LOOP('',(#3734,#3735,#3736,#3737));
#1015=EDGE_LOOP('',(#3738,#3739,#3740,#3741));
#1016=EDGE_LOOP('',(#3742,#3743,#3744,#3745));
#1017=EDGE_LOOP('',(#3746,#3747,#3748,#3749,#3750,#3751,#3752,#3753,#3754,
#3755,#3756,#3757,#3758,#3759,#3760,#3761,#3762,#3763,#3764,#3765,#3766,
#3767,#3768,#3769,#3770,#3771,#3772,#3773,#3774,#3775,#3776,#3777,#3778,
#3779,#3780));
#1018=EDGE_LOOP('',(#3781));
#1019=EDGE_LOOP('',(#3782));
#1020=EDGE_LOOP('',(#3783));
#1021=EDGE_LOOP('',(#3784));
#1022=EDGE_LOOP('',(#3785));
#1023=EDGE_LOOP('',(#3786));
#1024=EDGE_LOOP('',(#3787));
#1025=EDGE_LOOP('',(#3788,#3789,#3790,#3791));
#1026=EDGE_LOOP('',(#3792,#3793,#3794,#3795));
#1027=EDGE_LOOP('',(#3796,#3797,#3798,#3799));
#1028=EDGE_LOOP('',(#3800,#3801,#3802,#3803));
#1029=EDGE_LOOP('',(#3804,#3805,#3806,#3807));
#1030=EDGE_LOOP('',(#3808,#3809,#3810,#3811));
#1031=EDGE_LOOP('',(#3812,#3813,#3814,#3815));
#1032=EDGE_LOOP('',(#3816,#3817,#3818,#3819));
#1033=EDGE_LOOP('',(#3820,#3821,#3822,#3823));
#1034=EDGE_LOOP('',(#3824,#3825,#3826,#3827));
#1035=EDGE_LOOP('',(#3828,#3829,#3830,#3831));
#1036=EDGE_LOOP('',(#3832,#3833,#3834,#3835));
#1037=EDGE_LOOP('',(#3836,#3837,#3838,#3839));
#1038=EDGE_LOOP('',(#3840,#3841,#3842,#3843));
#1039=EDGE_LOOP('',(#3844,#3845,#3846,#3847));
#1040=EDGE_LOOP('',(#3848,#3849,#3850,#3851));
#1041=EDGE_LOOP('',(#3852,#3853,#3854,#3855));
#1042=EDGE_LOOP('',(#3856,#3857,#3858,#3859));
#1043=EDGE_LOOP('',(#3860,#3861,#3862,#3863));
#1044=EDGE_LOOP('',(#3864,#3865,#3866,#3867));
#1045=EDGE_LOOP('',(#3868,#3869,#3870,#3871));
#1046=EDGE_LOOP('',(#3872,#3873,#3874,#3875));
#1047=EDGE_LOOP('',(#3876,#3877,#3878,#3879));
#1048=EDGE_LOOP('',(#3880,#3881,#3882,#3883));
#1049=EDGE_LOOP('',(#3884,#3885,#3886,#3887));
#1050=EDGE_LOOP('',(#3888,#3889,#3890,#3891));
#1051=EDGE_LOOP('',(#3892,#3893,#3894,#3895));
#1052=EDGE_LOOP('',(#3896,#3897,#3898,#3899));
#1053=EDGE_LOOP('',(#3900,#3901,#3902,#3903));
#1054=EDGE_LOOP('',(#3904,#3905,#3906,#3907));
#1055=EDGE_LOOP('',(#3908,#3909,#3910,#3911));
#1056=EDGE_LOOP('',(#3912,#3913,#3914,#3915));
#1057=EDGE_LOOP('',(#3916,#3917,#3918,#3919));
#1058=EDGE_LOOP('',(#3920,#3921,#3922,#3923));
#1059=EDGE_LOOP('',(#3924,#3925,#3926,#3927));
#1060=EDGE_LOOP('',(#3928,#3929,#3930,#3931));
#1061=EDGE_LOOP('',(#3932,#3933,#3934,#3935));
#1062=EDGE_LOOP('',(#3936,#3937,#3938,#3939));
#1063=EDGE_LOOP('',(#3940,#3941,#3942,#3943));
#1064=EDGE_LOOP('',(#3944,#3945,#3946,#3947));
#1065=EDGE_LOOP('',(#3948,#3949,#3950,#3951));
#1066=EDGE_LOOP('',(#3952,#3953,#3954,#3955));
#1067=EDGE_LOOP('',(#3956,#3957,#3958,#3959));
#1068=EDGE_LOOP('',(#3960,#3961,#3962,#3963));
#1069=EDGE_LOOP('',(#3964,#3965,#3966,#3967));
#1070=EDGE_LOOP('',(#3968,#3969,#3970,#3971));
#1071=EDGE_LOOP('',(#3972,#3973,#3974,#3975));
#1072=EDGE_LOOP('',(#3976,#3977,#3978,#3979));
#1073=EDGE_LOOP('',(#3980,#3981,#3982,#3983));
#1074=EDGE_LOOP('',(#3984,#3985,#3986,#3987));
#1075=EDGE_LOOP('',(#3988,#3989,#3990,#3991));
#1076=EDGE_LOOP('',(#3992,#3993,#3994,#3995,#3996,#3997,#3998,#3999,#4000,
#4001,#4002,#4003,#4004,#4005,#4006,#4007,#4008,#4009,#4010,#4011,#4012,
#4013,#4014,#4015,#4016,#4017,#4018,#4019,#4020,#4021,#4022,#4023,#4024,
#4025,#4026));
#1077=EDGE_LOOP('',(#4027));
#1078=EDGE_LOOP('',(#4028));
#1079=EDGE_LOOP('',(#4029));
#1080=EDGE_LOOP('',(#4030,#4031,#4032,#4033,#4034,#4035,#4036,#4037));
#1081=EDGE_LOOP('',(#4038,#4039,#4040,#4041,#4042,#4043,#4044,#4045));
#1082=EDGE_LOOP('',(#4046,#4047,#4048,#4049,#4050,#4051,#4052,#4053));
#1083=EDGE_LOOP('',(#4054,#4055,#4056,#4057,#4058,#4059,#4060,#4061));
#1084=EDGE_LOOP('',(#4062,#4063,#4064,#4065,#4066,#4067,#4068,#4069));
#1085=EDGE_LOOP('',(#4070));
#1086=EDGE_LOOP('',(#4071,#4072,#4073,#4074,#4075,#4076,#4077,#4078));
#1087=EDGE_LOOP('',(#4079));
#1088=EDGE_LOOP('',(#4080,#4081,#4082,#4083,#4084,#4085,#4086,#4087));
#1089=EDGE_LOOP('',(#4088));
#1090=EDGE_LOOP('',(#4089,#4090,#4091,#4092,#4093,#4094,#4095,#4096));
#1091=EDGE_LOOP('',(#4097));
#1092=EDGE_LOOP('',(#4098,#4099,#4100,#4101));
#1093=EDGE_LOOP('',(#4102,#4103,#4104,#4105));
#1094=EDGE_LOOP('',(#4106,#4107,#4108,#4109));
#1095=EDGE_LOOP('',(#4110,#4111,#4112,#4113));
#1096=EDGE_LOOP('',(#4114,#4115,#4116,#4117));
#1097=EDGE_LOOP('',(#4118,#4119,#4120,#4121));
#1098=EDGE_LOOP('',(#4122,#4123,#4124,#4125));
#1099=EDGE_LOOP('',(#4126,#4127,#4128,#4129));
#1100=EDGE_LOOP('',(#4130,#4131,#4132,#4133));
#1101=EDGE_LOOP('',(#4134,#4135,#4136,#4137));
#1102=EDGE_LOOP('',(#4138,#4139,#4140,#4141));
#1103=EDGE_LOOP('',(#4142));
#1104=EDGE_LOOP('',(#4143,#4144,#4145,#4146));
#1105=EDGE_LOOP('',(#4147));
#1106=EDGE_LOOP('',(#4148,#4149,#4150,#4151));
#1107=EDGE_LOOP('',(#4152,#4153));
#1108=EDGE_LOOP('',(#4154,#4155,#4156,#4157,#4158));
#1109=EDGE_LOOP('',(#4159));
#1110=EDGE_LOOP('',(#4160,#4161,#4162));
#1111=EDGE_LOOP('',(#4163,#4164,#4165,#4166));
#1112=EDGE_LOOP('',(#4167,#4168,#4169,#4170));
#1113=EDGE_LOOP('',(#4171));
#1114=EDGE_LOOP('',(#4172));
#1115=EDGE_LOOP('',(#4173,#4174,#4175,#4176));
#1116=EDGE_LOOP('',(#4177,#4178,#4179,#4180));
#1117=EDGE_LOOP('',(#4181,#4182,#4183,#4184));
#1118=EDGE_LOOP('',(#4185,#4186,#4187,#4188));
#1119=EDGE_LOOP('',(#4189,#4190,#4191,#4192));
#1120=EDGE_LOOP('',(#4193,#4194,#4195,#4196));
#1121=EDGE_LOOP('',(#4197,#4198,#4199,#4200,#4201,#4202));
#1122=EDGE_LOOP('',(#4203,#4204,#4205,#4206));
#1123=EDGE_LOOP('',(#4207));
#1124=EDGE_LOOP('',(#4208,#4209,#4210,#4211,#4212,#4213));
#1125=EDGE_LOOP('',(#4214,#4215,#4216));
#1126=EDGE_LOOP('',(#4217,#4218,#4219,#4220,#4221,#4222,#4223,#4224,#4225,
#4226,#4227,#4228,#4229,#4230,#4231,#4232,#4233,#4234,#4235,#4236,#4237,
#4238,#4239,#4240,#4241,#4242,#4243,#4244));
#1127=EDGE_LOOP('',(#4245));
#1128=EDGE_LOOP('',(#4246));
#1129=EDGE_LOOP('',(#4247));
#1130=EDGE_LOOP('',(#4248));
#1131=EDGE_LOOP('',(#4249));
#1132=EDGE_LOOP('',(#4250));
#1133=EDGE_LOOP('',(#4251));
#1134=EDGE_LOOP('',(#4252));
#1135=EDGE_LOOP('',(#4253,#4254,#4255));
#1136=EDGE_LOOP('',(#4256,#4257,#4258));
#1137=EDGE_LOOP('',(#4259,#4260,#4261,#4262));
#1138=EDGE_LOOP('',(#4263,#4264,#4265,#4266));
#1139=EDGE_LOOP('',(#4267,#4268,#4269,#4270));
#1140=EDGE_LOOP('',(#4271,#4272,#4273,#4274));
#1141=EDGE_LOOP('',(#4275,#4276,#4277,#4278));
#1142=EDGE_LOOP('',(#4279,#4280,#4281,#4282));
#1143=EDGE_LOOP('',(#4283,#4284,#4285,#4286));
#1144=EDGE_LOOP('',(#4287,#4288,#4289,#4290));
#1145=EDGE_LOOP('',(#4291,#4292,#4293,#4294));
#1146=EDGE_LOOP('',(#4295,#4296,#4297,#4298,#4299,#4300,#4301,#4302,#4303,
#4304,#4305,#4306,#4307,#4308,#4309,#4310,#4311,#4312,#4313,#4314,#4315,
#4316,#4317,#4318,#4319,#4320,#4321,#4322));
#1147=EDGE_LOOP('',(#4323));
#1148=EDGE_LOOP('',(#4324));
#1149=EDGE_LOOP('',(#4325));
#1150=EDGE_LOOP('',(#4326));
#1151=EDGE_LOOP('',(#4327));
#1152=EDGE_LOOP('',(#4328,#4329,#4330,#4331));
#1153=EDGE_LOOP('',(#4332,#4333,#4334,#4335));
#1154=EDGE_LOOP('',(#4336,#4337,#4338,#4339));
#1155=EDGE_LOOP('',(#4340,#4341,#4342,#4343));
#1156=EDGE_LOOP('',(#4344,#4345,#4346,#4347));
#1157=EDGE_LOOP('',(#4348,#4349,#4350,#4351));
#1158=EDGE_LOOP('',(#4352,#4353,#4354,#4355));
#1159=EDGE_LOOP('',(#4356,#4357,#4358,#4359));
#1160=EDGE_LOOP('',(#4360,#4361,#4362,#4363));
#1161=EDGE_LOOP('',(#4364,#4365,#4366,#4367));
#1162=EDGE_LOOP('',(#4368,#4369,#4370,#4371));
#1163=EDGE_LOOP('',(#4372,#4373,#4374,#4375));
#1164=EDGE_LOOP('',(#4376,#4377,#4378,#4379));
#1165=EDGE_LOOP('',(#4380,#4381,#4382,#4383));
#1166=EDGE_LOOP('',(#4384,#4385,#4386,#4387));
#1167=EDGE_LOOP('',(#4388,#4389,#4390,#4391));
#1168=EDGE_LOOP('',(#4392,#4393,#4394,#4395));
#1169=EDGE_LOOP('',(#4396,#4397,#4398,#4399));
#1170=EDGE_LOOP('',(#4400,#4401,#4402,#4403));
#1171=EDGE_LOOP('',(#4404,#4405,#4406,#4407));
#1172=EDGE_LOOP('',(#4408,#4409,#4410,#4411));
#1173=EDGE_LOOP('',(#4412,#4413,#4414,#4415));
#1174=EDGE_LOOP('',(#4416,#4417,#4418,#4419));
#1175=EDGE_LOOP('',(#4420,#4421,#4422,#4423));
#1176=EDGE_LOOP('',(#4424,#4425,#4426,#4427));
#1177=EDGE_LOOP('',(#4428,#4429,#4430,#4431));
#1178=EDGE_LOOP('',(#4432,#4433,#4434,#4435));
#1179=EDGE_LOOP('',(#4436,#4437,#4438,#4439));
#1180=EDGE_LOOP('',(#4440,#4441,#4442,#4443));
#1181=EDGE_LOOP('',(#4444,#4445,#4446,#4447));
#1182=EDGE_LOOP('',(#4448,#4449,#4450,#4451));
#1183=EDGE_LOOP('',(#4452,#4453,#4454,#4455));
#1184=EDGE_LOOP('',(#4456,#4457,#4458,#4459));
#1185=EDGE_LOOP('',(#4460,#4461,#4462,#4463));
#1186=EDGE_LOOP('',(#4464,#4465,#4466,#4467));
#1187=EDGE_LOOP('',(#4468,#4469,#4470,#4471));
#1188=EDGE_LOOP('',(#4472,#4473,#4474,#4475));
#1189=EDGE_LOOP('',(#4476,#4477,#4478,#4479));
#1190=EDGE_LOOP('',(#4480,#4481,#4482,#4483));
#1191=EDGE_LOOP('',(#4484,#4485,#4486,#4487));
#1192=EDGE_LOOP('',(#4488,#4489,#4490,#4491));
#1193=EDGE_LOOP('',(#4492,#4493,#4494,#4495));
#1194=EDGE_LOOP('',(#4496,#4497,#4498,#4499));
#1195=EDGE_LOOP('',(#4500,#4501,#4502,#4503));
#1196=EDGE_LOOP('',(#4504,#4505,#4506,#4507));
#1197=EDGE_LOOP('',(#4508,#4509,#4510,#4511));
#1198=EDGE_LOOP('',(#4512,#4513,#4514,#4515));
#1199=EDGE_LOOP('',(#4516,#4517,#4518,#4519));
#1200=EDGE_LOOP('',(#4520,#4521,#4522,#4523));
#1201=EDGE_LOOP('',(#4524,#4525,#4526,#4527));
#1202=EDGE_LOOP('',(#4528,#4529,#4530,#4531));
#1203=EDGE_LOOP('',(#4532,#4533,#4534,#4535));
#1204=EDGE_LOOP('',(#4536,#4537,#4538,#4539));
#1205=EDGE_LOOP('',(#4540,#4541,#4542,#4543));
#1206=EDGE_LOOP('',(#4544,#4545,#4546,#4547));
#1207=EDGE_LOOP('',(#4548,#4549,#4550,#4551));
#1208=EDGE_LOOP('',(#4552,#4553,#4554,#4555));
#1209=EDGE_LOOP('',(#4556,#4557,#4558,#4559));
#1210=EDGE_LOOP('',(#4560,#4561,#4562,#4563));
#1211=EDGE_LOOP('',(#4564,#4565,#4566,#4567));
#1212=EDGE_LOOP('',(#4568,#4569,#4570,#4571));
#1213=EDGE_LOOP('',(#4572,#4573,#4574,#4575));
#1214=EDGE_LOOP('',(#4576,#4577,#4578,#4579));
#1215=EDGE_LOOP('',(#4580,#4581,#4582,#4583));
#1216=EDGE_LOOP('',(#4584,#4585,#4586,#4587));
#1217=EDGE_LOOP('',(#4588,#4589,#4590,#4591));
#1218=EDGE_LOOP('',(#4592,#4593,#4594,#4595));
#1219=EDGE_LOOP('',(#4596,#4597,#4598,#4599));
#1220=EDGE_LOOP('',(#4600,#4601,#4602,#4603));
#1221=EDGE_LOOP('',(#4604,#4605,#4606,#4607));
#1222=EDGE_LOOP('',(#4608,#4609,#4610,#4611));
#1223=EDGE_LOOP('',(#4612,#4613,#4614,#4615));
#1224=EDGE_LOOP('',(#4616,#4617,#4618,#4619));
#1225=EDGE_LOOP('',(#4620,#4621,#4622,#4623));
#1226=EDGE_LOOP('',(#4624,#4625,#4626,#4627));
#1227=EDGE_LOOP('',(#4628,#4629,#4630,#4631));
#1228=EDGE_LOOP('',(#4632,#4633,#4634,#4635));
#1229=EDGE_LOOP('',(#4636,#4637,#4638,#4639));
#1230=EDGE_LOOP('',(#4640,#4641,#4642,#4643));
#1231=EDGE_LOOP('',(#4644,#4645,#4646,#4647));
#1232=EDGE_LOOP('',(#4648,#4649,#4650,#4651));
#1233=EDGE_LOOP('',(#4652,#4653,#4654,#4655));
#1234=EDGE_LOOP('',(#4656,#4657,#4658,#4659));
#1235=EDGE_LOOP('',(#4660,#4661,#4662,#4663));
#1236=EDGE_LOOP('',(#4664,#4665,#4666,#4667));
#1237=EDGE_LOOP('',(#4668,#4669,#4670,#4671));
#1238=EDGE_LOOP('',(#4672,#4673,#4674,#4675));
#1239=EDGE_LOOP('',(#4676,#4677,#4678,#4679));
#1240=EDGE_LOOP('',(#4680,#4681,#4682,#4683));
#1241=EDGE_LOOP('',(#4684,#4685,#4686,#4687));
#1242=EDGE_LOOP('',(#4688));
#1243=EDGE_LOOP('',(#4689,#4690,#4691,#4692));
#1244=EDGE_LOOP('',(#4693));
#1245=EDGE_LOOP('',(#4694,#4695,#4696));
#1246=EDGE_LOOP('',(#4697,#4698,#4699,#4700));
#1247=EDGE_LOOP('',(#4701,#4702,#4703,#4704));
#1248=EDGE_LOOP('',(#4705));
#1249=EDGE_LOOP('',(#4706));
#1250=EDGE_LOOP('',(#4707,#4708,#4709,#4710));
#1251=EDGE_LOOP('',(#4711,#4712,#4713,#4714));
#1252=EDGE_LOOP('',(#4715,#4716,#4717,#4718));
#1253=EDGE_LOOP('',(#4719,#4720,#4721,#4722));
#1254=EDGE_LOOP('',(#4723,#4724,#4725,#4726));
#1255=EDGE_LOOP('',(#4727,#4728,#4729,#4730));
#1256=EDGE_LOOP('',(#4731,#4732,#4733,#4734,#4735,#4736));
#1257=EDGE_LOOP('',(#4737,#4738,#4739,#4740));
#1258=EDGE_LOOP('',(#4741));
#1259=EDGE_LOOP('',(#4742,#4743,#4744,#4745,#4746,#4747));
#1260=EDGE_LOOP('',(#4748,#4749,#4750,#4751));
#1261=EDGE_LOOP('',(#4752,#4753));
#1262=EDGE_LOOP('',(#4754,#4755,#4756,#4757,#4758));
#1263=EDGE_LOOP('',(#4759));
#1264=EDGE_LOOP('',(#4760,#4761,#4762,#4763));
#1265=EDGE_LOOP('',(#4764,#4765));
#1266=EDGE_LOOP('',(#4766,#4767,#4768,#4769,#4770));
#1267=EDGE_LOOP('',(#4771));
#1268=EDGE_LOOP('',(#4772,#4773,#4774,#4775));
#1269=EDGE_LOOP('',(#4776,#4777,#4778,#4779));
#1270=EDGE_LOOP('',(#4780));
#1271=EDGE_LOOP('',(#4781,#4782,#4783,#4784));
#1272=EDGE_LOOP('',(#4785));
#1273=EDGE_LOOP('',(#4786,#4787,#4788,#4789));
#1274=EDGE_LOOP('',(#4790,#4791));
#1275=EDGE_LOOP('',(#4792,#4793,#4794,#4795,#4796));
#1276=EDGE_LOOP('',(#4797));
#1277=EDGE_LOOP('',(#4798,#4799,#4800,#4801));
#1278=EDGE_LOOP('',(#4802,#4803,#4804,#4805));
#1279=EDGE_LOOP('',(#4806));
#1280=EDGE_LOOP('',(#4807,#4808,#4809,#4810));
#1281=EDGE_LOOP('',(#4811));
#1282=EDGE_LOOP('',(#4812,#4813,#4814));
#1283=EDGE_LOOP('',(#4815,#4816,#4817,#4818));
#1284=EDGE_LOOP('',(#4819,#4820,#4821,#4822));
#1285=EDGE_LOOP('',(#4823));
#1286=EDGE_LOOP('',(#4824));
#1287=EDGE_LOOP('',(#4825,#4826,#4827,#4828));
#1288=EDGE_LOOP('',(#4829,#4830,#4831,#4832));
#1289=EDGE_LOOP('',(#4833,#4834,#4835,#4836));
#1290=EDGE_LOOP('',(#4837,#4838,#4839,#4840));
#1291=EDGE_LOOP('',(#4841,#4842,#4843,#4844));
#1292=EDGE_LOOP('',(#4845,#4846,#4847,#4848));
#1293=EDGE_LOOP('',(#4849,#4850,#4851,#4852,#4853,#4854));
#1294=EDGE_LOOP('',(#4855,#4856,#4857,#4858));
#1295=EDGE_LOOP('',(#4859));
#1296=EDGE_LOOP('',(#4860,#4861,#4862,#4863,#4864,#4865));
#1297=LINE('',#7799,#1759);
#1298=LINE('',#7801,#1760);
#1299=LINE('',#7803,#1761);
#1300=LINE('',#7804,#1762);
#1301=LINE('',#7809,#1763);
#1302=LINE('',#7813,#1764);
#1303=LINE('',#7815,#1765);
#1304=LINE('',#7816,#1766);
#1305=LINE('',#7821,#1767);
#1306=LINE('',#7825,#1768);
#1307=LINE('',#7827,#1769);
#1308=LINE('',#7828,#1770);
#1309=LINE('',#7833,#1771);
#1310=LINE('',#7837,#1772);
#1311=LINE('',#7839,#1773);
#1312=LINE('',#7840,#1774);
#1313=LINE('',#7847,#1775);
#1314=LINE('',#7849,#1776);
#1315=LINE('',#7851,#1777);
#1316=LINE('',#7852,#1778);
#1317=LINE('',#7857,#1779);
#1318=LINE('',#7861,#1780);
#1319=LINE('',#7863,#1781);
#1320=LINE('',#7864,#1782);
#1321=LINE('',#7869,#1783);
#1322=LINE('',#7873,#1784);
#1323=LINE('',#7875,#1785);
#1324=LINE('',#7876,#1786);
#1325=LINE('',#7881,#1787);
#1326=LINE('',#7885,#1788);
#1327=LINE('',#7887,#1789);
#1328=LINE('',#7888,#1790);
#1329=LINE('',#7895,#1791);
#1330=LINE('',#7897,#1792);
#1331=LINE('',#7899,#1793);
#1332=LINE('',#7900,#1794);
#1333=LINE('',#7905,#1795);
#1334=LINE('',#7909,#1796);
#1335=LINE('',#7911,#1797);
#1336=LINE('',#7912,#1798);
#1337=LINE('',#7917,#1799);
#1338=LINE('',#7921,#1800);
#1339=LINE('',#7923,#1801);
#1340=LINE('',#7924,#1802);
#1341=LINE('',#7929,#1803);
#1342=LINE('',#7933,#1804);
#1343=LINE('',#7935,#1805);
#1344=LINE('',#7936,#1806);
#1345=LINE('',#7943,#1807);
#1346=LINE('',#7945,#1808);
#1347=LINE('',#7947,#1809);
#1348=LINE('',#7948,#1810);
#1349=LINE('',#7953,#1811);
#1350=LINE('',#7957,#1812);
#1351=LINE('',#7959,#1813);
#1352=LINE('',#7960,#1814);
#1353=LINE('',#7965,#1815);
#1354=LINE('',#7969,#1816);
#1355=LINE('',#7971,#1817);
#1356=LINE('',#7972,#1818);
#1357=LINE('',#7977,#1819);
#1358=LINE('',#7981,#1820);
#1359=LINE('',#7983,#1821);
#1360=LINE('',#7984,#1822);
#1361=LINE('',#7992,#1823);
#1362=LINE('',#7998,#1824);
#1363=LINE('',#8016,#1825);
#1364=LINE('',#8021,#1826);
#1365=LINE('',#8027,#1827);
#1366=LINE('',#8028,#1828);
#1367=LINE('',#8029,#1829);
#1368=LINE('',#8033,#1830);
#1369=LINE('',#8039,#1831);
#1370=LINE('',#8040,#1832);
#1371=LINE('',#8041,#1833);
#1372=LINE('',#8045,#1834);
#1373=LINE('',#8051,#1835);
#1374=LINE('',#8052,#1836);
#1375=LINE('',#8053,#1837);
#1376=LINE('',#8057,#1838);
#1377=LINE('',#8063,#1839);
#1378=LINE('',#8064,#1840);
#1379=LINE('',#8065,#1841);
#1380=LINE('',#8069,#1842);
#1381=LINE('',#8075,#1843);
#1382=LINE('',#8076,#1844);
#1383=LINE('',#8077,#1845);
#1384=LINE('',#8081,#1846);
#1385=LINE('',#8087,#1847);
#1386=LINE('',#8088,#1848);
#1387=LINE('',#8089,#1849);
#1388=LINE('',#8093,#1850);
#1389=LINE('',#8099,#1851);
#1390=LINE('',#8100,#1852);
#1391=LINE('',#8101,#1853);
#1392=LINE('',#8105,#1854);
#1393=LINE('',#8111,#1855);
#1394=LINE('',#8112,#1856);
#1395=LINE('',#8113,#1857);
#1396=LINE('',#8118,#1858);
#1397=LINE('',#8122,#1859);
#1398=LINE('',#8124,#1860);
#1399=LINE('',#8125,#1861);
#1400=LINE('',#8130,#1862);
#1401=LINE('',#8134,#1863);
#1402=LINE('',#8136,#1864);
#1403=LINE('',#8137,#1865);
#1404=LINE('',#8142,#1866);
#1405=LINE('',#8146,#1867);
#1406=LINE('',#8148,#1868);
#1407=LINE('',#8149,#1869);
#1408=LINE('',#8154,#1870);
#1409=LINE('',#8158,#1871);
#1410=LINE('',#8160,#1872);
#1411=LINE('',#8161,#1873);
#1412=LINE('',#8166,#1874);
#1413=LINE('',#8170,#1875);
#1414=LINE('',#8172,#1876);
#1415=LINE('',#8173,#1877);
#1416=LINE('',#8178,#1878);
#1417=LINE('',#8182,#1879);
#1418=LINE('',#8184,#1880);
#1419=LINE('',#8185,#1881);
#1420=LINE('',#8190,#1882);
#1421=LINE('',#8194,#1883);
#1422=LINE('',#8196,#1884);
#1423=LINE('',#8197,#1885);
#1424=LINE('',#8202,#1886);
#1425=LINE('',#8206,#1887);
#1426=LINE('',#8208,#1888);
#1427=LINE('',#8209,#1889);
#1428=LINE('',#8213,#1890);
#1429=LINE('',#8221,#1891);
#1430=LINE('',#8223,#1892);
#1431=LINE('',#8224,#1893);
#1432=LINE('',#8227,#1894);
#1433=LINE('',#8231,#1895);
#1434=LINE('',#8232,#1896);
#1435=LINE('',#8235,#1897);
#1436=LINE('',#8239,#1898);
#1437=LINE('',#8240,#1899);
#1438=LINE('',#8243,#1900);
#1439=LINE('',#8247,#1901);
#1440=LINE('',#8248,#1902);
#1441=LINE('',#8251,#1903);
#1442=LINE('',#8255,#1904);
#1443=LINE('',#8256,#1905);
#1444=LINE('',#8259,#1906);
#1445=LINE('',#8263,#1907);
#1446=LINE('',#8264,#1908);
#1447=LINE('',#8267,#1909);
#1448=LINE('',#8271,#1910);
#1449=LINE('',#8272,#1911);
#1450=LINE('',#8275,#1912);
#1451=LINE('',#8279,#1913);
#1452=LINE('',#8280,#1914);
#1453=LINE('',#8283,#1915);
#1454=LINE('',#8287,#1916);
#1455=LINE('',#8291,#1917);
#1456=LINE('',#8318,#1918);
#1457=LINE('',#8321,#1919);
#1458=LINE('',#8325,#1920);
#1459=LINE('',#8326,#1921);
#1460=LINE('',#8329,#1922);
#1461=LINE('',#8333,#1923);
#1462=LINE('',#8334,#1924);
#1463=LINE('',#8337,#1925);
#1464=LINE('',#8341,#1926);
#1465=LINE('',#8342,#1927);
#1466=LINE('',#8345,#1928);
#1467=LINE('',#8349,#1929);
#1468=LINE('',#8350,#1930);
#1469=LINE('',#8353,#1931);
#1470=LINE('',#8357,#1932);
#1471=LINE('',#8358,#1933);
#1472=LINE('',#8361,#1934);
#1473=LINE('',#8365,#1935);
#1474=LINE('',#8366,#1936);
#1475=LINE('',#8369,#1937);
#1476=LINE('',#8373,#1938);
#1477=LINE('',#8374,#1939);
#1478=LINE('',#8377,#1940);
#1479=LINE('',#8381,#1941);
#1480=LINE('',#8382,#1942);
#1481=LINE('',#8386,#1943);
#1482=LINE('',#8391,#1944);
#1483=LINE('',#8393,#1945);
#1484=LINE('',#8394,#1946);
#1485=LINE('',#8399,#1947);
#1486=LINE('',#8403,#1948);
#1487=LINE('',#8405,#1949);
#1488=LINE('',#8406,#1950);
#1489=LINE('',#8411,#1951);
#1490=LINE('',#8416,#1952);
#1491=LINE('',#8417,#1953);
#1492=LINE('',#8418,#1954);
#1493=LINE('',#8423,#1955);
#1494=LINE('',#8428,#1956);
#1495=LINE('',#8429,#1957);
#1496=LINE('',#8430,#1958);
#1497=LINE('',#8435,#1959);
#1498=LINE('',#8440,#1960);
#1499=LINE('',#8441,#1961);
#1500=LINE('',#8442,#1962);
#1501=LINE('',#8447,#1963);
#1502=LINE('',#8452,#1964);
#1503=LINE('',#8453,#1965);
#1504=LINE('',#8454,#1966);
#1505=LINE('',#8459,#1967);
#1506=LINE('',#8464,#1968);
#1507=LINE('',#8465,#1969);
#1508=LINE('',#8466,#1970);
#1509=LINE('',#8471,#1971);
#1510=LINE('',#8475,#1972);
#1511=LINE('',#8477,#1973);
#1512=LINE('',#8478,#1974);
#1513=LINE('',#8481,#1975);
#1514=LINE('',#8487,#1976);
#1515=LINE('',#8488,#1977);
#1516=LINE('',#8490,#1978);
#1517=LINE('',#8492,#1979);
#1518=LINE('',#8494,#1980);
#1519=LINE('',#8496,#1981);
#1520=LINE('',#8498,#1982);
#1521=LINE('',#8500,#1983);
#1522=LINE('',#8502,#1984);
#1523=LINE('',#8504,#1985);
#1524=LINE('',#8506,#1986);
#1525=LINE('',#8508,#1987);
#1526=LINE('',#8510,#1988);
#1527=LINE('',#8512,#1989);
#1528=LINE('',#8514,#1990);
#1529=LINE('',#8516,#1991);
#1530=LINE('',#8536,#1992);
#1531=LINE('',#8538,#1993);
#1532=LINE('',#8542,#1994);
#1533=LINE('',#8544,#1995);
#1534=LINE('',#8547,#1996);
#1535=LINE('',#8550,#1997);
#1536=LINE('',#8552,#1998);
#1537=LINE('',#8554,#1999);
#1538=LINE('',#8561,#2000);
#1539=LINE('',#8565,#2001);
#1540=LINE('',#8570,#2002);
#1541=LINE('',#9123,#2003);
#1542=LINE('',#9129,#2004);
#1543=LINE('',#9131,#2005);
#1544=LINE('',#9133,#2006);
#1545=LINE('',#9134,#2007);
#1546=LINE('',#9137,#2008);
#1547=LINE('',#9139,#2009);
#1548=LINE('',#9140,#2010);
#1549=LINE('',#9143,#2011);
#1550=LINE('',#9145,#2012);
#1551=LINE('',#9146,#2013);
#1552=LINE('',#9149,#2014);
#1553=LINE('',#9151,#2015);
#1554=LINE('',#9152,#2016);
#1555=LINE('',#9155,#2017);
#1556=LINE('',#9157,#2018);
#1557=LINE('',#9158,#2019);
#1558=LINE('',#9160,#2020);
#1559=LINE('',#9161,#2021);
#1560=LINE('',#9166,#2022);
#1561=LINE('',#9177,#2023);
#1562=LINE('',#9181,#2024);
#1563=LINE('',#9185,#2025);
#1564=LINE('',#9189,#2026);
#1565=LINE('',#9193,#2027);
#1566=LINE('',#9197,#2028);
#1567=LINE('',#9201,#2029);
#1568=LINE('',#9207,#2030);
#1569=LINE('',#9211,#2031);
#1570=LINE('',#9215,#2032);
#1571=LINE('',#9221,#2033);
#1572=LINE('',#9225,#2034);
#1573=LINE('',#9229,#2035);
#1574=LINE('',#9253,#2036);
#1575=LINE('',#9258,#2037);
#1576=LINE('',#9261,#2038);
#1577=LINE('',#9266,#2039);
#1578=LINE('',#9270,#2040);
#1579=LINE('',#9274,#2041);
#1580=LINE('',#9278,#2042);
#1581=LINE('',#9282,#2043);
#1582=LINE('',#9285,#2044);
#1583=LINE('',#9290,#2045);
#1584=LINE('',#9294,#2046);
#1585=LINE('',#9298,#2047);
#1586=LINE('',#9302,#2048);
#1587=LINE('',#9308,#2049);
#1588=LINE('',#9312,#2050);
#1589=LINE('',#9316,#2051);
#1590=LINE('',#9322,#2052);
#1591=LINE('',#9326,#2053);
#1592=LINE('',#9330,#2054);
#1593=LINE('',#9334,#2055);
#1594=LINE('',#9338,#2056);
#1595=LINE('',#9342,#2057);
#1596=LINE('',#9353,#2058);
#1597=LINE('',#9355,#2059);
#1598=LINE('',#9357,#2060);
#1599=LINE('',#9360,#2061);
#1600=LINE('',#9362,#2062);
#1601=LINE('',#9363,#2063);
#1602=LINE('',#9367,#2064);
#1603=LINE('',#9370,#2065);
#1604=LINE('',#9371,#2066);
#1605=LINE('',#9375,#2067);
#1606=LINE('',#9378,#2068);
#1607=LINE('',#9379,#2069);
#1608=LINE('',#9383,#2070);
#1609=LINE('',#9386,#2071);
#1610=LINE('',#9387,#2072);
#1611=LINE('',#9390,#2073);
#1612=LINE('',#9395,#2074);
#1613=LINE('',#9398,#2075);
#1614=LINE('',#9399,#2076);
#1615=LINE('',#9403,#2077);
#1616=LINE('',#9406,#2078);
#1617=LINE('',#9407,#2079);
#1618=LINE('',#9411,#2080);
#1619=LINE('',#9414,#2081);
#1620=LINE('',#9415,#2082);
#1621=LINE('',#9419,#2083);
#1622=LINE('',#9423,#2084);
#1623=LINE('',#9426,#2085);
#1624=LINE('',#9427,#2086);
#1625=LINE('',#9431,#2087);
#1626=LINE('',#9434,#2088);
#1627=LINE('',#9435,#2089);
#1628=LINE('',#9439,#2090);
#1629=LINE('',#9442,#2091);
#1630=LINE('',#9443,#2092);
#1631=LINE('',#9447,#2093);
#1632=LINE('',#9450,#2094);
#1633=LINE('',#9451,#2095);
#1634=LINE('',#9455,#2096);
#1635=LINE('',#9458,#2097);
#1636=LINE('',#9459,#2098);
#1637=LINE('',#9463,#2099);
#1638=LINE('',#9466,#2100);
#1639=LINE('',#9467,#2101);
#1640=LINE('',#9472,#2102);
#1641=LINE('',#9474,#2103);
#1642=LINE('',#9475,#2104);
#1643=LINE('',#9478,#2105);
#1644=LINE('',#9482,#2106);
#1645=LINE('',#9483,#2107);
#1646=LINE('',#9486,#2108);
#1647=LINE('',#9490,#2109);
#1648=LINE('',#9491,#2110);
#1649=LINE('',#9494,#2111);
#1650=LINE('',#9498,#2112);
#1651=LINE('',#9502,#2113);
#1652=LINE('',#9503,#2114);
#1653=LINE('',#9506,#2115);
#1654=LINE('',#9510,#2116);
#1655=LINE('',#9511,#2117);
#1656=LINE('',#9514,#2118);
#1657=LINE('',#9518,#2119);
#1658=LINE('',#9519,#2120);
#1659=LINE('',#9522,#2121);
#1660=LINE('',#9526,#2122);
#1661=LINE('',#9527,#2123);
#1662=LINE('',#9529,#2124);
#1663=LINE('',#9530,#2125);
#1664=LINE('',#9532,#2126);
#1665=LINE('',#9534,#2127);
#1666=LINE('',#9536,#2128);
#1667=LINE('',#9538,#2129);
#1668=LINE('',#9540,#2130);
#1669=LINE('',#9542,#2131);
#1670=LINE('',#9544,#2132);
#1671=LINE('',#9546,#2133);
#1672=LINE('',#9548,#2134);
#1673=LINE('',#9550,#2135);
#1674=LINE('',#9552,#2136);
#1675=LINE('',#9554,#2137);
#1676=LINE('',#9556,#2138);
#1677=LINE('',#9559,#2139);
#1678=LINE('',#9563,#2140);
#1679=LINE('',#9567,#2141);
#1680=LINE('',#9568,#2142);
#1681=LINE('',#9571,#2143);
#1682=LINE('',#9575,#2144);
#1683=LINE('',#9576,#2145);
#1684=LINE('',#9579,#2146);
#1685=LINE('',#9583,#2147);
#1686=LINE('',#9584,#2148);
#1687=LINE('',#9587,#2149);
#1688=LINE('',#9591,#2150);
#1689=LINE('',#9592,#2151);
#1690=LINE('',#9595,#2152);
#1691=LINE('',#9599,#2153);
#1692=LINE('',#9600,#2154);
#1693=LINE('',#9603,#2155);
#1694=LINE('',#9607,#2156);
#1695=LINE('',#9608,#2157);
#1696=LINE('',#9612,#2158);
#1697=LINE('',#9613,#2159);
#1698=LINE('',#9615,#2160);
#1699=LINE('',#9617,#2161);
#1700=LINE('',#9619,#2162);
#1701=LINE('',#9621,#2163);
#1702=LINE('',#9623,#2164);
#1703=LINE('',#9625,#2165);
#1704=LINE('',#9627,#2166);
#1705=LINE('',#9629,#2167);
#1706=LINE('',#9631,#2168);
#1707=LINE('',#9633,#2169);
#1708=LINE('',#9635,#2170);
#1709=LINE('',#9639,#2171);
#1710=LINE('',#9645,#2172);
#1711=LINE('',#9649,#2173);
#1712=LINE('',#9654,#2174);
#1713=LINE('',#9671,#2175);
#1714=LINE('',#9677,#2176);
#1715=LINE('',#9679,#2177);
#1716=LINE('',#9681,#2178);
#1717=LINE('',#9682,#2179);
#1718=LINE('',#9685,#2180);
#1719=LINE('',#9687,#2181);
#1720=LINE('',#9688,#2182);
#1721=LINE('',#9691,#2183);
#1722=LINE('',#9693,#2184);
#1723=LINE('',#9694,#2185);
#1724=LINE('',#9697,#2186);
#1725=LINE('',#9699,#2187);
#1726=LINE('',#9700,#2188);
#1727=LINE('',#9703,#2189);
#1728=LINE('',#9705,#2190);
#1729=LINE('',#9706,#2191);
#1730=LINE('',#9708,#2192);
#1731=LINE('',#9709,#2193);
#1732=LINE('',#9714,#2194);
#1733=LINE('',#10793,#2195);
#1734=LINE('',#10797,#2196);
#1735=LINE('',#10802,#2197);
#1736=LINE('',#11272,#2198);
#1737=LINE('',#11276,#2199);
#1738=LINE('',#11281,#2200);
#1739=LINE('',#11298,#2201);
#1740=LINE('',#11304,#2202);
#1741=LINE('',#11306,#2203);
#1742=LINE('',#11308,#2204);
#1743=LINE('',#11309,#2205);
#1744=LINE('',#11312,#2206);
#1745=LINE('',#11314,#2207);
#1746=LINE('',#11315,#2208);
#1747=LINE('',#11318,#2209);
#1748=LINE('',#11320,#2210);
#1749=LINE('',#11321,#2211);
#1750=LINE('',#11324,#2212);
#1751=LINE('',#11326,#2213);
#1752=LINE('',#11327,#2214);
#1753=LINE('',#11330,#2215);
#1754=LINE('',#11332,#2216);
#1755=LINE('',#11333,#2217);
#1756=LINE('',#11335,#2218);
#1757=LINE('',#11336,#2219);
#1758=LINE('',#11341,#2220);
#1759=VECTOR('',#6116,10.);
#1760=VECTOR('',#6117,10.);
#1761=VECTOR('',#6118,10.);
#1762=VECTOR('',#6119,10.);
#1763=VECTOR('',#6124,10.);
#1764=VECTOR('',#6129,10.);
#1765=VECTOR('',#6130,10.);
#1766=VECTOR('',#6131,10.);
#1767=VECTOR('',#6136,10.);
#1768=VECTOR('',#6141,10.);
#1769=VECTOR('',#6142,10.);
#1770=VECTOR('',#6143,10.);
#1771=VECTOR('',#6148,10.);
#1772=VECTOR('',#6153,10.);
#1773=VECTOR('',#6154,10.);
#1774=VECTOR('',#6155,10.);
#1775=VECTOR('',#6164,10.);
#1776=VECTOR('',#6165,10.);
#1777=VECTOR('',#6166,10.);
#1778=VECTOR('',#6167,10.);
#1779=VECTOR('',#6172,10.);
#1780=VECTOR('',#6177,10.);
#1781=VECTOR('',#6178,10.);
#1782=VECTOR('',#6179,10.);
#1783=VECTOR('',#6184,10.);
#1784=VECTOR('',#6189,10.);
#1785=VECTOR('',#6190,10.);
#1786=VECTOR('',#6191,10.);
#1787=VECTOR('',#6196,10.);
#1788=VECTOR('',#6201,10.);
#1789=VECTOR('',#6202,10.);
#1790=VECTOR('',#6203,10.);
#1791=VECTOR('',#6212,10.);
#1792=VECTOR('',#6213,10.);
#1793=VECTOR('',#6214,10.);
#1794=VECTOR('',#6215,10.);
#1795=VECTOR('',#6220,10.);
#1796=VECTOR('',#6225,10.);
#1797=VECTOR('',#6226,10.);
#1798=VECTOR('',#6227,10.);
#1799=VECTOR('',#6232,10.);
#1800=VECTOR('',#6237,10.);
#1801=VECTOR('',#6238,10.);
#1802=VECTOR('',#6239,10.);
#1803=VECTOR('',#6244,10.);
#1804=VECTOR('',#6249,10.);
#1805=VECTOR('',#6250,10.);
#1806=VECTOR('',#6251,10.);
#1807=VECTOR('',#6260,10.);
#1808=VECTOR('',#6261,10.);
#1809=VECTOR('',#6262,10.);
#1810=VECTOR('',#6263,10.);
#1811=VECTOR('',#6268,10.);
#1812=VECTOR('',#6273,10.);
#1813=VECTOR('',#6274,10.);
#1814=VECTOR('',#6275,10.);
#1815=VECTOR('',#6280,10.);
#1816=VECTOR('',#6285,10.);
#1817=VECTOR('',#6286,10.);
#1818=VECTOR('',#6287,10.);
#1819=VECTOR('',#6292,10.);
#1820=VECTOR('',#6297,10.);
#1821=VECTOR('',#6298,10.);
#1822=VECTOR('',#6299,10.);
#1823=VECTOR('',#6310,1.77957176368631);
#1824=VECTOR('',#6317,1.77957176368631);
#1825=VECTOR('',#6324,10.);
#1826=VECTOR('',#6329,10.);
#1827=VECTOR('',#6336,10.);
#1828=VECTOR('',#6337,10.);
#1829=VECTOR('',#6338,10.);
#1830=VECTOR('',#6341,10.);
#1831=VECTOR('',#6348,10.);
#1832=VECTOR('',#6349,10.);
#1833=VECTOR('',#6350,10.);
#1834=VECTOR('',#6353,10.);
#1835=VECTOR('',#6360,10.);
#1836=VECTOR('',#6361,10.);
#1837=VECTOR('',#6362,10.);
#1838=VECTOR('',#6365,10.);
#1839=VECTOR('',#6372,10.);
#1840=VECTOR('',#6373,10.);
#1841=VECTOR('',#6374,10.);
#1842=VECTOR('',#6377,10.);
#1843=VECTOR('',#6384,10.);
#1844=VECTOR('',#6385,10.);
#1845=VECTOR('',#6386,10.);
#1846=VECTOR('',#6389,10.);
#1847=VECTOR('',#6396,10.);
#1848=VECTOR('',#6397,10.);
#1849=VECTOR('',#6398,10.);
#1850=VECTOR('',#6401,10.);
#1851=VECTOR('',#6408,10.);
#1852=VECTOR('',#6409,10.);
#1853=VECTOR('',#6410,10.);
#1854=VECTOR('',#6413,10.);
#1855=VECTOR('',#6420,10.);
#1856=VECTOR('',#6421,10.);
#1857=VECTOR('',#6422,10.);
#1858=VECTOR('',#6427,10.);
#1859=VECTOR('',#6432,10.);
#1860=VECTOR('',#6433,10.);
#1861=VECTOR('',#6434,10.);
#1862=VECTOR('',#6439,10.);
#1863=VECTOR('',#6444,10.);
#1864=VECTOR('',#6445,10.);
#1865=VECTOR('',#6446,10.);
#1866=VECTOR('',#6451,10.);
#1867=VECTOR('',#6456,10.);
#1868=VECTOR('',#6457,10.);
#1869=VECTOR('',#6458,10.);
#1870=VECTOR('',#6463,10.);
#1871=VECTOR('',#6468,10.);
#1872=VECTOR('',#6469,10.);
#1873=VECTOR('',#6470,10.);
#1874=VECTOR('',#6475,10.);
#1875=VECTOR('',#6480,10.);
#1876=VECTOR('',#6481,10.);
#1877=VECTOR('',#6482,10.);
#1878=VECTOR('',#6487,10.);
#1879=VECTOR('',#6492,10.);
#1880=VECTOR('',#6493,10.);
#1881=VECTOR('',#6494,10.);
#1882=VECTOR('',#6499,10.);
#1883=VECTOR('',#6504,10.);
#1884=VECTOR('',#6505,10.);
#1885=VECTOR('',#6506,10.);
#1886=VECTOR('',#6511,10.);
#1887=VECTOR('',#6516,10.);
#1888=VECTOR('',#6517,10.);
#1889=VECTOR('',#6518,10.);
#1890=VECTOR('',#6521,10.);
#1891=VECTOR('',#6534,10.);
#1892=VECTOR('',#6535,10.);
#1893=VECTOR('',#6536,10.);
#1894=VECTOR('',#6539,10.);
#1895=VECTOR('',#6544,10.);
#1896=VECTOR('',#6545,10.);
#1897=VECTOR('',#6548,10.);
#1898=VECTOR('',#6553,10.);
#1899=VECTOR('',#6554,10.);
#1900=VECTOR('',#6557,10.);
#1901=VECTOR('',#6562,10.);
#1902=VECTOR('',#6563,10.);
#1903=VECTOR('',#6566,10.);
#1904=VECTOR('',#6571,10.);
#1905=VECTOR('',#6572,10.);
#1906=VECTOR('',#6575,10.);
#1907=VECTOR('',#6580,10.);
#1908=VECTOR('',#6581,10.);
#1909=VECTOR('',#6584,10.);
#1910=VECTOR('',#6589,10.);
#1911=VECTOR('',#6590,10.);
#1912=VECTOR('',#6593,10.);
#1913=VECTOR('',#6598,10.);
#1914=VECTOR('',#6599,10.);
#1915=VECTOR('',#6602,10.);
#1916=VECTOR('',#6607,10.);
#1917=VECTOR('',#6612,10.);
#1918=VECTOR('',#6631,10.);
#1919=VECTOR('',#6634,10.);
#1920=VECTOR('',#6639,10.);
#1921=VECTOR('',#6640,10.);
#1922=VECTOR('',#6643,10.);
#1923=VECTOR('',#6648,10.);
#1924=VECTOR('',#6649,10.);
#1925=VECTOR('',#6652,10.);
#1926=VECTOR('',#6657,10.);
#1927=VECTOR('',#6658,10.);
#1928=VECTOR('',#6661,10.);
#1929=VECTOR('',#6666,10.);
#1930=VECTOR('',#6667,10.);
#1931=VECTOR('',#6670,10.);
#1932=VECTOR('',#6675,10.);
#1933=VECTOR('',#6676,10.);
#1934=VECTOR('',#6679,10.);
#1935=VECTOR('',#6684,10.);
#1936=VECTOR('',#6685,10.);
#1937=VECTOR('',#6688,10.);
#1938=VECTOR('',#6693,10.);
#1939=VECTOR('',#6694,10.);
#1940=VECTOR('',#6697,10.);
#1941=VECTOR('',#6702,10.);
#1942=VECTOR('',#6703,10.);
#1943=VECTOR('',#6706,10.);
#1944=VECTOR('',#6713,10.);
#1945=VECTOR('',#6714,10.);
#1946=VECTOR('',#6715,10.);
#1947=VECTOR('',#6720,10.);
#1948=VECTOR('',#6725,10.);
#1949=VECTOR('',#6726,10.);
#1950=VECTOR('',#6727,10.);
#1951=VECTOR('',#6732,10.);
#1952=VECTOR('',#6737,10.);
#1953=VECTOR('',#6738,10.);
#1954=VECTOR('',#6739,10.);
#1955=VECTOR('',#6744,10.);
#1956=VECTOR('',#6749,10.);
#1957=VECTOR('',#6750,10.);
#1958=VECTOR('',#6751,10.);
#1959=VECTOR('',#6756,10.);
#1960=VECTOR('',#6761,10.);
#1961=VECTOR('',#6762,10.);
#1962=VECTOR('',#6763,10.);
#1963=VECTOR('',#6768,10.);
#1964=VECTOR('',#6773,10.);
#1965=VECTOR('',#6774,10.);
#1966=VECTOR('',#6775,10.);
#1967=VECTOR('',#6780,10.);
#1968=VECTOR('',#6785,10.);
#1969=VECTOR('',#6786,10.);
#1970=VECTOR('',#6787,10.);
#1971=VECTOR('',#6792,10.);
#1972=VECTOR('',#6797,10.);
#1973=VECTOR('',#6798,10.);
#1974=VECTOR('',#6799,10.);
#1975=VECTOR('',#6802,10.);
#1976=VECTOR('',#6813,10.);
#1977=VECTOR('',#6814,10.);
#1978=VECTOR('',#6817,10.);
#1979=VECTOR('',#6820,10.);
#1980=VECTOR('',#6823,10.);
#1981=VECTOR('',#6826,10.);
#1982=VECTOR('',#6829,10.);
#1983=VECTOR('',#6832,10.);
#1984=VECTOR('',#6835,10.);
#1985=VECTOR('',#6838,10.);
#1986=VECTOR('',#6841,10.);
#1987=VECTOR('',#6844,10.);
#1988=VECTOR('',#6847,10.);
#1989=VECTOR('',#6850,10.);
#1990=VECTOR('',#6853,10.);
#1991=VECTOR('',#6856,10.);
#1992=VECTOR('',#6883,3.40761552865316);
#1993=VECTOR('',#6886,3.15761552865316);
#1994=VECTOR('',#6891,3.40761552865316);
#1995=VECTOR('',#6894,3.15761552865316);
#1996=VECTOR('',#6897,3.40761552865316);
#1997=VECTOR('',#6902,3.15761552865316);
#1998=VECTOR('',#6905,1.77957176368631);
#1999=VECTOR('',#6908,1.77957176368631);
#2000=VECTOR('',#6917,0.7);
#2001=VECTOR('',#6922,0.75);
#2002=VECTOR('',#6929,0.7);
#2003=VECTOR('',#6966,3.15761552865316);
#2004=VECTOR('',#6973,10.);
#2005=VECTOR('',#6974,10.);
#2006=VECTOR('',#6975,10.);
#2007=VECTOR('',#6976,10.);
#2008=VECTOR('',#6979,10.);
#2009=VECTOR('',#6980,10.);
#2010=VECTOR('',#6981,10.);
#2011=VECTOR('',#6984,10.);
#2012=VECTOR('',#6985,10.);
#2013=VECTOR('',#6986,10.);
#2014=VECTOR('',#6989,10.);
#2015=VECTOR('',#6990,10.);
#2016=VECTOR('',#6991,10.);
#2017=VECTOR('',#6994,10.);
#2018=VECTOR('',#6995,10.);
#2019=VECTOR('',#6996,10.);
#2020=VECTOR('',#6999,10.);
#2021=VECTOR('',#7000,10.);
#2022=VECTOR('',#7007,2.90761552865316);
#2023=VECTOR('',#7020,10.);
#2024=VECTOR('',#7023,10.);
#2025=VECTOR('',#7026,10.);
#2026=VECTOR('',#7029,10.);
#2027=VECTOR('',#7032,10.);
#2028=VECTOR('',#7035,10.);
#2029=VECTOR('',#7038,10.);
#2030=VECTOR('',#7043,10.);
#2031=VECTOR('',#7046,10.);
#2032=VECTOR('',#7049,10.);
#2033=VECTOR('',#7054,10.);
#2034=VECTOR('',#7057,10.);
#2035=VECTOR('',#7060,10.);
#2036=VECTOR('',#7087,1.5);
#2037=VECTOR('',#7094,1.25);
#2038=VECTOR('',#7097,1.5);
#2039=VECTOR('',#7104,1.25);
#2040=VECTOR('',#7109,1.5);
#2041=VECTOR('',#7114,1.25);
#2042=VECTOR('',#7119,1.5);
#2043=VECTOR('',#7124,1.25);
#2044=VECTOR('',#7127,1.5);
#2045=VECTOR('',#7132,10.);
#2046=VECTOR('',#7135,10.);
#2047=VECTOR('',#7138,10.);
#2048=VECTOR('',#7141,10.);
#2049=VECTOR('',#7146,10.);
#2050=VECTOR('',#7149,10.);
#2051=VECTOR('',#7152,10.);
#2052=VECTOR('',#7157,10.);
#2053=VECTOR('',#7160,10.);
#2054=VECTOR('',#7163,10.);
#2055=VECTOR('',#7166,10.);
#2056=VECTOR('',#7169,10.);
#2057=VECTOR('',#7172,10.);
#2058=VECTOR('',#7185,1.5);
#2059=VECTOR('',#7188,1.5);
#2060=VECTOR('',#7191,1.5);
#2061=VECTOR('',#7194,10.);
#2062=VECTOR('',#7195,10.);
#2063=VECTOR('',#7196,10.);
#2064=VECTOR('',#7201,10.);
#2065=VECTOR('',#7204,10.);
#2066=VECTOR('',#7205,10.);
#2067=VECTOR('',#7210,10.);
#2068=VECTOR('',#7213,10.);
#2069=VECTOR('',#7214,10.);
#2070=VECTOR('',#7219,10.);
#2071=VECTOR('',#7222,10.);
#2072=VECTOR('',#7223,10.);
#2073=VECTOR('',#7226,10.);
#2074=VECTOR('',#7233,10.);
#2075=VECTOR('',#7236,10.);
#2076=VECTOR('',#7237,10.);
#2077=VECTOR('',#7242,10.);
#2078=VECTOR('',#7245,10.);
#2079=VECTOR('',#7246,10.);
#2080=VECTOR('',#7251,10.);
#2081=VECTOR('',#7254,10.);
#2082=VECTOR('',#7255,10.);
#2083=VECTOR('',#7260,10.);
#2084=VECTOR('',#7265,10.);
#2085=VECTOR('',#7268,10.);
#2086=VECTOR('',#7269,10.);
#2087=VECTOR('',#7274,10.);
#2088=VECTOR('',#7277,10.);
#2089=VECTOR('',#7278,10.);
#2090=VECTOR('',#7283,10.);
#2091=VECTOR('',#7286,10.);
#2092=VECTOR('',#7287,10.);
#2093=VECTOR('',#7292,10.);
#2094=VECTOR('',#7295,10.);
#2095=VECTOR('',#7296,10.);
#2096=VECTOR('',#7301,10.);
#2097=VECTOR('',#7304,10.);
#2098=VECTOR('',#7305,10.);
#2099=VECTOR('',#7310,10.);
#2100=VECTOR('',#7313,10.);
#2101=VECTOR('',#7314,10.);
#2102=VECTOR('',#7321,10.);
#2103=VECTOR('',#7322,10.);
#2104=VECTOR('',#7323,10.);
#2105=VECTOR('',#7326,10.);
#2106=VECTOR('',#7331,10.);
#2107=VECTOR('',#7332,10.);
#2108=VECTOR('',#7335,10.);
#2109=VECTOR('',#7340,10.);
#2110=VECTOR('',#7341,10.);
#2111=VECTOR('',#7344,10.);
#2112=VECTOR('',#7349,10.);
#2113=VECTOR('',#7354,10.);
#2114=VECTOR('',#7355,10.);
#2115=VECTOR('',#7358,10.);
#2116=VECTOR('',#7363,10.);
#2117=VECTOR('',#7364,10.);
#2118=VECTOR('',#7367,10.);
#2119=VECTOR('',#7372,10.);
#2120=VECTOR('',#7373,10.);
#2121=VECTOR('',#7376,10.);
#2122=VECTOR('',#7381,10.);
#2123=VECTOR('',#7382,10.);
#2124=VECTOR('',#7385,10.);
#2125=VECTOR('',#7386,10.);
#2126=VECTOR('',#7389,10.);
#2127=VECTOR('',#7392,10.);
#2128=VECTOR('',#7395,10.);
#2129=VECTOR('',#7398,10.);
#2130=VECTOR('',#7401,10.);
#2131=VECTOR('',#7404,10.);
#2132=VECTOR('',#7407,10.);
#2133=VECTOR('',#7410,10.);
#2134=VECTOR('',#7413,10.);
#2135=VECTOR('',#7416,10.);
#2136=VECTOR('',#7419,10.);
#2137=VECTOR('',#7422,10.);
#2138=VECTOR('',#7425,10.);
#2139=VECTOR('',#7428,10.);
#2140=VECTOR('',#7433,10.);
#2141=VECTOR('',#7438,10.);
#2142=VECTOR('',#7439,10.);
#2143=VECTOR('',#7442,10.);
#2144=VECTOR('',#7447,10.);
#2145=VECTOR('',#7448,10.);
#2146=VECTOR('',#7451,10.);
#2147=VECTOR('',#7456,10.);
#2148=VECTOR('',#7457,10.);
#2149=VECTOR('',#7460,10.);
#2150=VECTOR('',#7465,10.);
#2151=VECTOR('',#7466,10.);
#2152=VECTOR('',#7469,10.);
#2153=VECTOR('',#7474,10.);
#2154=VECTOR('',#7475,10.);
#2155=VECTOR('',#7478,10.);
#2156=VECTOR('',#7483,10.);
#2157=VECTOR('',#7484,10.);
#2158=VECTOR('',#7491,10.);
#2159=VECTOR('',#7492,10.);
#2160=VECTOR('',#7495,10.);
#2161=VECTOR('',#7498,10.);
#2162=VECTOR('',#7501,10.);
#2163=VECTOR('',#7504,10.);
#2164=VECTOR('',#7507,10.);
#2165=VECTOR('',#7510,10.);
#2166=VECTOR('',#7513,10.);
#2167=VECTOR('',#7516,10.);
#2168=VECTOR('',#7519,10.);
#2169=VECTOR('',#7522,10.);
#2170=VECTOR('',#7525,10.);
#2171=VECTOR('',#7532,6.);
#2172=VECTOR('',#7539,0.7);
#2173=VECTOR('',#7544,0.75);
#2174=VECTOR('',#7551,0.7);
#2175=VECTOR('',#7574,3.15761552865316);
#2176=VECTOR('',#7581,10.);
#2177=VECTOR('',#7582,10.);
#2178=VECTOR('',#7583,10.);
#2179=VECTOR('',#7584,10.);
#2180=VECTOR('',#7587,10.);
#2181=VECTOR('',#7588,10.);
#2182=VECTOR('',#7589,10.);
#2183=VECTOR('',#7592,10.);
#2184=VECTOR('',#7593,10.);
#2185=VECTOR('',#7594,10.);
#2186=VECTOR('',#7597,10.);
#2187=VECTOR('',#7598,10.);
#2188=VECTOR('',#7599,10.);
#2189=VECTOR('',#7602,10.);
#2190=VECTOR('',#7603,10.);
#2191=VECTOR('',#7604,10.);
#2192=VECTOR('',#7607,10.);
#2193=VECTOR('',#7608,10.);
#2194=VECTOR('',#7615,2.90761552865316);
#2195=VECTOR('',#7652,0.7);
#2196=VECTOR('',#7657,0.75);
#2197=VECTOR('',#7664,0.7);
#2198=VECTOR('',#7689,0.699999999999999);
#2199=VECTOR('',#7694,0.75);
#2200=VECTOR('',#7701,0.7);
#2201=VECTOR('',#7724,3.15761552865316);
#2202=VECTOR('',#7731,10.);
#2203=VECTOR('',#7732,10.);
#2204=VECTOR('',#7733,10.);
#2205=VECTOR('',#7734,10.);
#2206=VECTOR('',#7737,10.);
#2207=VECTOR('',#7738,10.);
#2208=VECTOR('',#7739,10.);
#2209=VECTOR('',#7742,10.);
#2210=VECTOR('',#7743,10.);
#2211=VECTOR('',#7744,10.);
#2212=VECTOR('',#7747,10.);
#2213=VECTOR('',#7748,10.);
#2214=VECTOR('',#7749,10.);
#2215=VECTOR('',#7752,10.);
#2216=VECTOR('',#7753,10.);
#2217=VECTOR('',#7754,10.);
#2218=VECTOR('',#7757,10.);
#2219=VECTOR('',#7758,10.);
#2220=VECTOR('',#7765,2.90761552865316);
#2221=VERTEX_POINT('',#7797);
#2222=VERTEX_POINT('',#7798);
#2223=VERTEX_POINT('',#7800);
#2224=VERTEX_POINT('',#7802);
#2225=VERTEX_POINT('',#7806);
#2226=VERTEX_POINT('',#7808);
#2227=VERTEX_POINT('',#7812);
#2228=VERTEX_POINT('',#7814);
#2229=VERTEX_POINT('',#7818);
#2230=VERTEX_POINT('',#7820);
#2231=VERTEX_POINT('',#7824);
#2232=VERTEX_POINT('',#7826);
#2233=VERTEX_POINT('',#7830);
#2234=VERTEX_POINT('',#7832);
#2235=VERTEX_POINT('',#7836);
#2236=VERTEX_POINT('',#7838);
#2237=VERTEX_POINT('',#7845);
#2238=VERTEX_POINT('',#7846);
#2239=VERTEX_POINT('',#7848);
#2240=VERTEX_POINT('',#7850);
#2241=VERTEX_POINT('',#7854);
#2242=VERTEX_POINT('',#7856);
#2243=VERTEX_POINT('',#7860);
#2244=VERTEX_POINT('',#7862);
#2245=VERTEX_POINT('',#7866);
#2246=VERTEX_POINT('',#7868);
#2247=VERTEX_POINT('',#7872);
#2248=VERTEX_POINT('',#7874);
#2249=VERTEX_POINT('',#7878);
#2250=VERTEX_POINT('',#7880);
#2251=VERTEX_POINT('',#7884);
#2252=VERTEX_POINT('',#7886);
#2253=VERTEX_POINT('',#7893);
#2254=VERTEX_POINT('',#7894);
#2255=VERTEX_POINT('',#7896);
#2256=VERTEX_POINT('',#7898);
#2257=VERTEX_POINT('',#7902);
#2258=VERTEX_POINT('',#7904);
#2259=VERTEX_POINT('',#7908);
#2260=VERTEX_POINT('',#7910);
#2261=VERTEX_POINT('',#7914);
#2262=VERTEX_POINT('',#7916);
#2263=VERTEX_POINT('',#7920);
#2264=VERTEX_POINT('',#7922);
#2265=VERTEX_POINT('',#7926);
#2266=VERTEX_POINT('',#7928);
#2267=VERTEX_POINT('',#7932);
#2268=VERTEX_POINT('',#7934);
#2269=VERTEX_POINT('',#7941);
#2270=VERTEX_POINT('',#7942);
#2271=VERTEX_POINT('',#7944);
#2272=VERTEX_POINT('',#7946);
#2273=VERTEX_POINT('',#7950);
#2274=VERTEX_POINT('',#7952);
#2275=VERTEX_POINT('',#7956);
#2276=VERTEX_POINT('',#7958);
#2277=VERTEX_POINT('',#7962);
#2278=VERTEX_POINT('',#7964);
#2279=VERTEX_POINT('',#7968);
#2280=VERTEX_POINT('',#7970);
#2281=VERTEX_POINT('',#7974);
#2282=VERTEX_POINT('',#7976);
#2283=VERTEX_POINT('',#7980);
#2284=VERTEX_POINT('',#7982);
#2285=VERTEX_POINT('',#7989);
#2286=VERTEX_POINT('',#7991);
#2287=VERTEX_POINT('',#7995);
#2288=VERTEX_POINT('',#7997);
#2289=VERTEX_POINT('',#8001);
#2290=VERTEX_POINT('',#8002);
#2291=VERTEX_POINT('',#8013);
#2292=VERTEX_POINT('',#8015);
#2293=VERTEX_POINT('',#8019);
#2294=VERTEX_POINT('',#8020);
#2295=VERTEX_POINT('',#8025);
#2296=VERTEX_POINT('',#8026);
#2297=VERTEX_POINT('',#8031);
#2298=VERTEX_POINT('',#8032);
#2299=VERTEX_POINT('',#8037);
#2300=VERTEX_POINT('',#8038);
#2301=VERTEX_POINT('',#8043);
#2302=VERTEX_POINT('',#8044);
#2303=VERTEX_POINT('',#8049);
#2304=VERTEX_POINT('',#8050);
#2305=VERTEX_POINT('',#8055);
#2306=VERTEX_POINT('',#8056);
#2307=VERTEX_POINT('',#8061);
#2308=VERTEX_POINT('',#8062);
#2309=VERTEX_POINT('',#8067);
#2310=VERTEX_POINT('',#8068);
#2311=VERTEX_POINT('',#8073);
#2312=VERTEX_POINT('',#8074);
#2313=VERTEX_POINT('',#8079);
#2314=VERTEX_POINT('',#8080);
#2315=VERTEX_POINT('',#8085);
#2316=VERTEX_POINT('',#8086);
#2317=VERTEX_POINT('',#8091);
#2318=VERTEX_POINT('',#8092);
#2319=VERTEX_POINT('',#8097);
#2320=VERTEX_POINT('',#8098);
#2321=VERTEX_POINT('',#8103);
#2322=VERTEX_POINT('',#8104);
#2323=VERTEX_POINT('',#8109);
#2324=VERTEX_POINT('',#8110);
#2325=VERTEX_POINT('',#8115);
#2326=VERTEX_POINT('',#8117);
#2327=VERTEX_POINT('',#8121);
#2328=VERTEX_POINT('',#8123);
#2329=VERTEX_POINT('',#8127);
#2330=VERTEX_POINT('',#8129);
#2331=VERTEX_POINT('',#8133);
#2332=VERTEX_POINT('',#8135);
#2333=VERTEX_POINT('',#8139);
#2334=VERTEX_POINT('',#8141);
#2335=VERTEX_POINT('',#8145);
#2336=VERTEX_POINT('',#8147);
#2337=VERTEX_POINT('',#8151);
#2338=VERTEX_POINT('',#8153);
#2339=VERTEX_POINT('',#8157);
#2340=VERTEX_POINT('',#8159);
#2341=VERTEX_POINT('',#8163);
#2342=VERTEX_POINT('',#8165);
#2343=VERTEX_POINT('',#8169);
#2344=VERTEX_POINT('',#8171);
#2345=VERTEX_POINT('',#8175);
#2346=VERTEX_POINT('',#8177);
#2347=VERTEX_POINT('',#8181);
#2348=VERTEX_POINT('',#8183);
#2349=VERTEX_POINT('',#8187);
#2350=VERTEX_POINT('',#8189);
#2351=VERTEX_POINT('',#8193);
#2352=VERTEX_POINT('',#8195);
#2353=VERTEX_POINT('',#8199);
#2354=VERTEX_POINT('',#8201);
#2355=VERTEX_POINT('',#8205);
#2356=VERTEX_POINT('',#8207);
#2357=VERTEX_POINT('',#8211);
#2358=VERTEX_POINT('',#8212);
#2359=VERTEX_POINT('',#8220);
#2360=VERTEX_POINT('',#8222);
#2361=VERTEX_POINT('',#8226);
#2362=VERTEX_POINT('',#8230);
#2363=VERTEX_POINT('',#8234);
#2364=VERTEX_POINT('',#8238);
#2365=VERTEX_POINT('',#8242);
#2366=VERTEX_POINT('',#8246);
#2367=VERTEX_POINT('',#8250);
#2368=VERTEX_POINT('',#8254);
#2369=VERTEX_POINT('',#8258);
#2370=VERTEX_POINT('',#8262);
#2371=VERTEX_POINT('',#8266);
#2372=VERTEX_POINT('',#8270);
#2373=VERTEX_POINT('',#8274);
#2374=VERTEX_POINT('',#8278);
#2375=VERTEX_POINT('',#8282);
#2376=VERTEX_POINT('',#8286);
#2377=VERTEX_POINT('',#8290);
#2378=VERTEX_POINT('',#8294);
#2379=VERTEX_POINT('',#8296);
#2380=VERTEX_POINT('',#8298);
#2381=VERTEX_POINT('',#8300);
#2382=VERTEX_POINT('',#8302);
#2383=VERTEX_POINT('',#8305);
#2384=VERTEX_POINT('',#8316);
#2385=VERTEX_POINT('',#8320);
#2386=VERTEX_POINT('',#8324);
#2387=VERTEX_POINT('',#8328);
#2388=VERTEX_POINT('',#8332);
#2389=VERTEX_POINT('',#8336);
#2390=VERTEX_POINT('',#8340);
#2391=VERTEX_POINT('',#8344);
#2392=VERTEX_POINT('',#8348);
#2393=VERTEX_POINT('',#8352);
#2394=VERTEX_POINT('',#8356);
#2395=VERTEX_POINT('',#8360);
#2396=VERTEX_POINT('',#8364);
#2397=VERTEX_POINT('',#8368);
#2398=VERTEX_POINT('',#8372);
#2399=VERTEX_POINT('',#8376);
#2400=VERTEX_POINT('',#8380);
#2401=VERTEX_POINT('',#8384);
#2402=VERTEX_POINT('',#8385);
#2403=VERTEX_POINT('',#8390);
#2404=VERTEX_POINT('',#8392);
#2405=VERTEX_POINT('',#8396);
#2406=VERTEX_POINT('',#8398);
#2407=VERTEX_POINT('',#8402);
#2408=VERTEX_POINT('',#8404);
#2409=VERTEX_POINT('',#8408);
#2410=VERTEX_POINT('',#8410);
#2411=VERTEX_POINT('',#8414);
#2412=VERTEX_POINT('',#8415);
#2413=VERTEX_POINT('',#8420);
#2414=VERTEX_POINT('',#8422);
#2415=VERTEX_POINT('',#8426);
#2416=VERTEX_POINT('',#8427);
#2417=VERTEX_POINT('',#8432);
#2418=VERTEX_POINT('',#8434);
#2419=VERTEX_POINT('',#8438);
#2420=VERTEX_POINT('',#8439);
#2421=VERTEX_POINT('',#8444);
#2422=VERTEX_POINT('',#8446);
#2423=VERTEX_POINT('',#8450);
#2424=VERTEX_POINT('',#8451);
#2425=VERTEX_POINT('',#8456);
#2426=VERTEX_POINT('',#8458);
#2427=VERTEX_POINT('',#8462);
#2428=VERTEX_POINT('',#8463);
#2429=VERTEX_POINT('',#8468);
#2430=VERTEX_POINT('',#8470);
#2431=VERTEX_POINT('',#8474);
#2432=VERTEX_POINT('',#8476);
#2433=VERTEX_POINT('',#8480);
#2434=VERTEX_POINT('',#8519);
#2435=VERTEX_POINT('',#8521);
#2436=VERTEX_POINT('',#8523);
#2437=VERTEX_POINT('',#8526);
#2438=VERTEX_POINT('',#8531);
#2439=VERTEX_POINT('',#8534);
#2440=VERTEX_POINT('',#8540);
#2441=VERTEX_POINT('',#8546);
#2442=VERTEX_POINT('',#8558);
#2443=VERTEX_POINT('',#8560);
#2444=VERTEX_POINT('',#8564);
#2445=VERTEX_POINT('',#8569);
#2446=VERTEX_POINT('',#8575);
#2447=VERTEX_POINT('',#8578);
#2448=VERTEX_POINT('',#8579);
#2449=VERTEX_POINT('',#9069);
#2450=VERTEX_POINT('',#9111);
#2451=VERTEX_POINT('',#9113);
#2452=VERTEX_POINT('',#9116);
#2453=VERTEX_POINT('',#9118);
#2454=VERTEX_POINT('',#9122);
#2455=VERTEX_POINT('',#9127);
#2456=VERTEX_POINT('',#9128);
#2457=VERTEX_POINT('',#9130);
#2458=VERTEX_POINT('',#9132);
#2459=VERTEX_POINT('',#9136);
#2460=VERTEX_POINT('',#9138);
#2461=VERTEX_POINT('',#9142);
#2462=VERTEX_POINT('',#9144);
#2463=VERTEX_POINT('',#9148);
#2464=VERTEX_POINT('',#9150);
#2465=VERTEX_POINT('',#9154);
#2466=VERTEX_POINT('',#9156);
#2467=VERTEX_POINT('',#9164);
#2468=VERTEX_POINT('',#9170);
#2469=VERTEX_POINT('',#9172);
#2470=VERTEX_POINT('',#9175);
#2471=VERTEX_POINT('',#9176);
#2472=VERTEX_POINT('',#9178);
#2473=VERTEX_POINT('',#9180);
#2474=VERTEX_POINT('',#9182);
#2475=VERTEX_POINT('',#9184);
#2476=VERTEX_POINT('',#9186);
#2477=VERTEX_POINT('',#9188);
#2478=VERTEX_POINT('',#9190);
#2479=VERTEX_POINT('',#9192);
#2480=VERTEX_POINT('',#9194);
#2481=VERTEX_POINT('',#9196);
#2482=VERTEX_POINT('',#9198);
#2483=VERTEX_POINT('',#9200);
#2484=VERTEX_POINT('',#9202);
#2485=VERTEX_POINT('',#9204);
#2486=VERTEX_POINT('',#9206);
#2487=VERTEX_POINT('',#9208);
#2488=VERTEX_POINT('',#9210);
#2489=VERTEX_POINT('',#9212);
#2490=VERTEX_POINT('',#9214);
#2491=VERTEX_POINT('',#9216);
#2492=VERTEX_POINT('',#9218);
#2493=VERTEX_POINT('',#9220);
#2494=VERTEX_POINT('',#9222);
#2495=VERTEX_POINT('',#9224);
#2496=VERTEX_POINT('',#9226);
#2497=VERTEX_POINT('',#9228);
#2498=VERTEX_POINT('',#9231);
#2499=VERTEX_POINT('',#9233);
#2500=VERTEX_POINT('',#9235);
#2501=VERTEX_POINT('',#9237);
#2502=VERTEX_POINT('',#9239);
#2503=VERTEX_POINT('',#9241);
#2504=VERTEX_POINT('',#9243);
#2505=VERTEX_POINT('',#9246);
#2506=VERTEX_POINT('',#9249);
#2507=VERTEX_POINT('',#9252);
#2508=VERTEX_POINT('',#9256);
#2509=VERTEX_POINT('',#9260);
#2510=VERTEX_POINT('',#9264);
#2511=VERTEX_POINT('',#9268);
#2512=VERTEX_POINT('',#9272);
#2513=VERTEX_POINT('',#9276);
#2514=VERTEX_POINT('',#9280);
#2515=VERTEX_POINT('',#9284);
#2516=VERTEX_POINT('',#9288);
#2517=VERTEX_POINT('',#9289);
#2518=VERTEX_POINT('',#9291);
#2519=VERTEX_POINT('',#9293);
#2520=VERTEX_POINT('',#9295);
#2521=VERTEX_POINT('',#9297);
#2522=VERTEX_POINT('',#9299);
#2523=VERTEX_POINT('',#9301);
#2524=VERTEX_POINT('',#9303);
#2525=VERTEX_POINT('',#9305);
#2526=VERTEX_POINT('',#9307);
#2527=VERTEX_POINT('',#9309);
#2528=VERTEX_POINT('',#9311);
#2529=VERTEX_POINT('',#9313);
#2530=VERTEX_POINT('',#9315);
#2531=VERTEX_POINT('',#9317);
#2532=VERTEX_POINT('',#9319);
#2533=VERTEX_POINT('',#9321);
#2534=VERTEX_POINT('',#9323);
#2535=VERTEX_POINT('',#9325);
#2536=VERTEX_POINT('',#9327);
#2537=VERTEX_POINT('',#9329);
#2538=VERTEX_POINT('',#9331);
#2539=VERTEX_POINT('',#9333);
#2540=VERTEX_POINT('',#9335);
#2541=VERTEX_POINT('',#9337);
#2542=VERTEX_POINT('',#9339);
#2543=VERTEX_POINT('',#9341);
#2544=VERTEX_POINT('',#9344);
#2545=VERTEX_POINT('',#9346);
#2546=VERTEX_POINT('',#9348);
#2547=VERTEX_POINT('',#9350);
#2548=VERTEX_POINT('',#9359);
#2549=VERTEX_POINT('',#9361);
#2550=VERTEX_POINT('',#9365);
#2551=VERTEX_POINT('',#9369);
#2552=VERTEX_POINT('',#9373);
#2553=VERTEX_POINT('',#9377);
#2554=VERTEX_POINT('',#9381);
#2555=VERTEX_POINT('',#9385);
#2556=VERTEX_POINT('',#9389);
#2557=VERTEX_POINT('',#9393);
#2558=VERTEX_POINT('',#9397);
#2559=VERTEX_POINT('',#9401);
#2560=VERTEX_POINT('',#9405);
#2561=VERTEX_POINT('',#9409);
#2562=VERTEX_POINT('',#9413);
#2563=VERTEX_POINT('',#9417);
#2564=VERTEX_POINT('',#9421);
#2565=VERTEX_POINT('',#9425);
#2566=VERTEX_POINT('',#9429);
#2567=VERTEX_POINT('',#9433);
#2568=VERTEX_POINT('',#9437);
#2569=VERTEX_POINT('',#9441);
#2570=VERTEX_POINT('',#9445);
#2571=VERTEX_POINT('',#9449);
#2572=VERTEX_POINT('',#9453);
#2573=VERTEX_POINT('',#9457);
#2574=VERTEX_POINT('',#9461);
#2575=VERTEX_POINT('',#9465);
#2576=VERTEX_POINT('',#9471);
#2577=VERTEX_POINT('',#9473);
#2578=VERTEX_POINT('',#9477);
#2579=VERTEX_POINT('',#9481);
#2580=VERTEX_POINT('',#9485);
#2581=VERTEX_POINT('',#9489);
#2582=VERTEX_POINT('',#9493);
#2583=VERTEX_POINT('',#9497);
#2584=VERTEX_POINT('',#9501);
#2585=VERTEX_POINT('',#9505);
#2586=VERTEX_POINT('',#9509);
#2587=VERTEX_POINT('',#9513);
#2588=VERTEX_POINT('',#9517);
#2589=VERTEX_POINT('',#9521);
#2590=VERTEX_POINT('',#9525);
#2591=VERTEX_POINT('',#9558);
#2592=VERTEX_POINT('',#9562);
#2593=VERTEX_POINT('',#9566);
#2594=VERTEX_POINT('',#9570);
#2595=VERTEX_POINT('',#9574);
#2596=VERTEX_POINT('',#9578);
#2597=VERTEX_POINT('',#9582);
#2598=VERTEX_POINT('',#9586);
#2599=VERTEX_POINT('',#9590);
#2600=VERTEX_POINT('',#9594);
#2601=VERTEX_POINT('',#9598);
#2602=VERTEX_POINT('',#9602);
#2603=VERTEX_POINT('',#9606);
#2604=VERTEX_POINT('',#9642);
#2605=VERTEX_POINT('',#9644);
#2606=VERTEX_POINT('',#9648);
#2607=VERTEX_POINT('',#9653);
#2608=VERTEX_POINT('',#9659);
#2609=VERTEX_POINT('',#9661);
#2610=VERTEX_POINT('',#9664);
#2611=VERTEX_POINT('',#9666);
#2612=VERTEX_POINT('',#9670);
#2613=VERTEX_POINT('',#9675);
#2614=VERTEX_POINT('',#9676);
#2615=VERTEX_POINT('',#9678);
#2616=VERTEX_POINT('',#9680);
#2617=VERTEX_POINT('',#9684);
#2618=VERTEX_POINT('',#9686);
#2619=VERTEX_POINT('',#9690);
#2620=VERTEX_POINT('',#9692);
#2621=VERTEX_POINT('',#9696);
#2622=VERTEX_POINT('',#9698);
#2623=VERTEX_POINT('',#9702);
#2624=VERTEX_POINT('',#9704);
#2625=VERTEX_POINT('',#9712);
#2626=VERTEX_POINT('',#9718);
#2627=VERTEX_POINT('',#9721);
#2628=VERTEX_POINT('',#9722);
#2629=VERTEX_POINT('',#10212);
#2630=VERTEX_POINT('',#10254);
#2631=VERTEX_POINT('',#10257);
#2632=VERTEX_POINT('',#10258);
#2633=VERTEX_POINT('',#10748);
#2634=VERTEX_POINT('',#10790);
#2635=VERTEX_POINT('',#10792);
#2636=VERTEX_POINT('',#10796);
#2637=VERTEX_POINT('',#10801);
#2638=VERTEX_POINT('',#10807);
#2639=VERTEX_POINT('',#10810);
#2640=VERTEX_POINT('',#10811);
#2641=VERTEX_POINT('',#11227);
#2642=VERTEX_POINT('',#11269);
#2643=VERTEX_POINT('',#11271);
#2644=VERTEX_POINT('',#11275);
#2645=VERTEX_POINT('',#11280);
#2646=VERTEX_POINT('',#11286);
#2647=VERTEX_POINT('',#11288);
#2648=VERTEX_POINT('',#11291);
#2649=VERTEX_POINT('',#11293);
#2650=VERTEX_POINT('',#11297);
#2651=VERTEX_POINT('',#11302);
#2652=VERTEX_POINT('',#11303);
#2653=VERTEX_POINT('',#11305);
#2654=VERTEX_POINT('',#11307);
#2655=VERTEX_POINT('',#11311);
#2656=VERTEX_POINT('',#11313);
#2657=VERTEX_POINT('',#11317);
#2658=VERTEX_POINT('',#11319);
#2659=VERTEX_POINT('',#11323);
#2660=VERTEX_POINT('',#11325);
#2661=VERTEX_POINT('',#11329);
#2662=VERTEX_POINT('',#11331);
#2663=VERTEX_POINT('',#11339);
#2664=EDGE_CURVE('',#2221,#2222,#1297,.T.);
#2665=EDGE_CURVE('',#2221,#2223,#1298,.T.);
#2666=EDGE_CURVE('',#2223,#2224,#1299,.T.);
#2667=EDGE_CURVE('',#2222,#2224,#1300,.T.);
#2668=EDGE_CURVE('',#2225,#2221,#273,.T.);
#2669=EDGE_CURVE('',#2225,#2226,#1301,.T.);
#2670=EDGE_CURVE('',#2226,#2223,#274,.T.);
#2671=EDGE_CURVE('',#2227,#2225,#1302,.T.);
#2672=EDGE_CURVE('',#2227,#2228,#1303,.T.);
#2673=EDGE_CURVE('',#2228,#2226,#1304,.T.);
#2674=EDGE_CURVE('',#2229,#2227,#275,.T.);
#2675=EDGE_CURVE('',#2229,#2230,#1305,.T.);
#2676=EDGE_CURVE('',#2230,#2228,#276,.T.);
#2677=EDGE_CURVE('',#2231,#2229,#1306,.T.);
#2678=EDGE_CURVE('',#2231,#2232,#1307,.T.);
#2679=EDGE_CURVE('',#2232,#2230,#1308,.T.);
#2680=EDGE_CURVE('',#2233,#2231,#277,.T.);
#2681=EDGE_CURVE('',#2233,#2234,#1309,.T.);
#2682=EDGE_CURVE('',#2234,#2232,#278,.T.);
#2683=EDGE_CURVE('',#2235,#2233,#1310,.T.);
#2684=EDGE_CURVE('',#2235,#2236,#1311,.T.);
#2685=EDGE_CURVE('',#2236,#2234,#1312,.T.);
#2686=EDGE_CURVE('',#2222,#2235,#279,.T.);
#2687=EDGE_CURVE('',#2224,#2236,#280,.T.);
#2688=EDGE_CURVE('',#2237,#2238,#1313,.T.);
#2689=EDGE_CURVE('',#2237,#2239,#1314,.T.);
#2690=EDGE_CURVE('',#2239,#2240,#1315,.T.);
#2691=EDGE_CURVE('',#2238,#2240,#1316,.T.);
#2692=EDGE_CURVE('',#2241,#2237,#281,.T.);
#2693=EDGE_CURVE('',#2241,#2242,#1317,.T.);
#2694=EDGE_CURVE('',#2242,#2239,#282,.T.);
#2695=EDGE_CURVE('',#2243,#2241,#1318,.T.);
#2696=EDGE_CURVE('',#2243,#2244,#1319,.T.);
#2697=EDGE_CURVE('',#2244,#2242,#1320,.T.);
#2698=EDGE_CURVE('',#2245,#2243,#283,.T.);
#2699=EDGE_CURVE('',#2245,#2246,#1321,.T.);
#2700=EDGE_CURVE('',#2246,#2244,#284,.T.);
#2701=EDGE_CURVE('',#2247,#2245,#1322,.T.);
#2702=EDGE_CURVE('',#2247,#2248,#1323,.T.);
#2703=EDGE_CURVE('',#2248,#2246,#1324,.T.);
#2704=EDGE_CURVE('',#2249,#2247,#285,.T.);
#2705=EDGE_CURVE('',#2249,#2250,#1325,.T.);
#2706=EDGE_CURVE('',#2250,#2248,#286,.T.);
#2707=EDGE_CURVE('',#2251,#2249,#1326,.T.);
#2708=EDGE_CURVE('',#2251,#2252,#1327,.T.);
#2709=EDGE_CURVE('',#2252,#2250,#1328,.T.);
#2710=EDGE_CURVE('',#2238,#2251,#287,.T.);
#2711=EDGE_CURVE('',#2240,#2252,#288,.T.);
#2712=EDGE_CURVE('',#2253,#2254,#1329,.T.);
#2713=EDGE_CURVE('',#2253,#2255,#1330,.T.);
#2714=EDGE_CURVE('',#2255,#2256,#1331,.T.);
#2715=EDGE_CURVE('',#2254,#2256,#1332,.T.);
#2716=EDGE_CURVE('',#2257,#2253,#289,.T.);
#2717=EDGE_CURVE('',#2257,#2258,#1333,.T.);
#2718=EDGE_CURVE('',#2258,#2255,#290,.T.);
#2719=EDGE_CURVE('',#2259,#2257,#1334,.T.);
#2720=EDGE_CURVE('',#2259,#2260,#1335,.T.);
#2721=EDGE_CURVE('',#2260,#2258,#1336,.T.);
#2722=EDGE_CURVE('',#2261,#2259,#291,.T.);
#2723=EDGE_CURVE('',#2261,#2262,#1337,.T.);
#2724=EDGE_CURVE('',#2262,#2260,#292,.T.);
#2725=EDGE_CURVE('',#2263,#2261,#1338,.T.);
#2726=EDGE_CURVE('',#2263,#2264,#1339,.T.);
#2727=EDGE_CURVE('',#2264,#2262,#1340,.T.);
#2728=EDGE_CURVE('',#2265,#2263,#293,.T.);
#2729=EDGE_CURVE('',#2265,#2266,#1341,.T.);
#2730=EDGE_CURVE('',#2266,#2264,#294,.T.);
#2731=EDGE_CURVE('',#2267,#2265,#1342,.T.);
#2732=EDGE_CURVE('',#2267,#2268,#1343,.T.);
#2733=EDGE_CURVE('',#2268,#2266,#1344,.T.);
#2734=EDGE_CURVE('',#2254,#2267,#295,.T.);
#2735=EDGE_CURVE('',#2256,#2268,#296,.T.);
#2736=EDGE_CURVE('',#2269,#2270,#1345,.T.);
#2737=EDGE_CURVE('',#2269,#2271,#1346,.T.);
#2738=EDGE_CURVE('',#2271,#2272,#1347,.T.);
#2739=EDGE_CURVE('',#2270,#2272,#1348,.T.);
#2740=EDGE_CURVE('',#2273,#2269,#297,.T.);
#2741=EDGE_CURVE('',#2273,#2274,#1349,.T.);
#2742=EDGE_CURVE('',#2274,#2271,#298,.T.);
#2743=EDGE_CURVE('',#2275,#2273,#1350,.T.);
#2744=EDGE_CURVE('',#2275,#2276,#1351,.T.);
#2745=EDGE_CURVE('',#2276,#2274,#1352,.T.);
#2746=EDGE_CURVE('',#2277,#2275,#299,.T.);
#2747=EDGE_CURVE('',#2277,#2278,#1353,.T.);
#2748=EDGE_CURVE('',#2278,#2276,#300,.T.);
#2749=EDGE_CURVE('',#2279,#2277,#1354,.T.);
#2750=EDGE_CURVE('',#2279,#2280,#1355,.T.);
#2751=EDGE_CURVE('',#2280,#2278,#1356,.T.);
#2752=EDGE_CURVE('',#2281,#2279,#301,.T.);
#2753=EDGE_CURVE('',#2281,#2282,#1357,.T.);
#2754=EDGE_CURVE('',#2282,#2280,#302,.T.);
#2755=EDGE_CURVE('',#2283,#2281,#1358,.T.);
#2756=EDGE_CURVE('',#2283,#2284,#1359,.T.);
#2757=EDGE_CURVE('',#2284,#2282,#1360,.T.);
#2758=EDGE_CURVE('',#2270,#2283,#303,.T.);
#2759=EDGE_CURVE('',#2272,#2284,#304,.T.);
#2760=EDGE_CURVE('',#2285,#2285,#305,.T.);
#2761=EDGE_CURVE('',#2285,#2286,#1361,.T.);
#2762=EDGE_CURVE('',#2286,#2286,#306,.T.);
#2763=EDGE_CURVE('',#2287,#2287,#307,.T.);
#2764=EDGE_CURVE('',#2287,#2288,#1362,.T.);
#2765=EDGE_CURVE('',#2288,#2288,#308,.T.);
#2766=EDGE_CURVE('',#2289,#2290,#173,.T.);
#2767=EDGE_CURVE('',#2290,#2291,#309,.T.);
#2768=EDGE_CURVE('',#2291,#2292,#1363,.T.);
#2769=EDGE_CURVE('',#2292,#2289,#310,.T.);
#2770=EDGE_CURVE('',#2293,#2294,#1364,.T.);
#2771=EDGE_CURVE('',#2294,#2292,#311,.T.);
#2772=EDGE_CURVE('',#2291,#2293,#312,.T.);
#2773=EDGE_CURVE('',#2295,#2296,#1365,.T.);
#2774=EDGE_CURVE('',#2296,#2294,#1366,.T.);
#2775=EDGE_CURVE('',#2293,#2295,#1367,.T.);
#2776=EDGE_CURVE('',#2297,#2298,#1368,.T.);
#2777=EDGE_CURVE('',#2298,#2296,#313,.T.);
#2778=EDGE_CURVE('',#2295,#2297,#314,.T.);
#2779=EDGE_CURVE('',#2299,#2300,#1369,.T.);
#2780=EDGE_CURVE('',#2300,#2298,#1370,.T.);
#2781=EDGE_CURVE('',#2297,#2299,#1371,.T.);
#2782=EDGE_CURVE('',#2301,#2302,#1372,.T.);
#2783=EDGE_CURVE('',#2302,#2300,#315,.T.);
#2784=EDGE_CURVE('',#2299,#2301,#316,.T.);
#2785=EDGE_CURVE('',#2303,#2304,#1373,.T.);
#2786=EDGE_CURVE('',#2304,#2302,#1374,.T.);
#2787=EDGE_CURVE('',#2301,#2303,#1375,.T.);
#2788=EDGE_CURVE('',#2305,#2306,#1376,.T.);
#2789=EDGE_CURVE('',#2306,#2304,#317,.T.);
#2790=EDGE_CURVE('',#2303,#2305,#318,.T.);
#2791=EDGE_CURVE('',#2307,#2308,#1377,.T.);
#2792=EDGE_CURVE('',#2308,#2306,#1378,.T.);
#2793=EDGE_CURVE('',#2305,#2307,#1379,.T.);
#2794=EDGE_CURVE('',#2309,#2310,#1380,.T.);
#2795=EDGE_CURVE('',#2310,#2308,#319,.T.);
#2796=EDGE_CURVE('',#2307,#2309,#320,.T.);
#2797=EDGE_CURVE('',#2311,#2312,#1381,.T.);
#2798=EDGE_CURVE('',#2312,#2310,#1382,.T.);
#2799=EDGE_CURVE('',#2309,#2311,#1383,.T.);
#2800=EDGE_CURVE('',#2313,#2314,#1384,.T.);
#2801=EDGE_CURVE('',#2314,#2312,#321,.T.);
#2802=EDGE_CURVE('',#2311,#2313,#322,.T.);
#2803=EDGE_CURVE('',#2315,#2316,#1385,.T.);
#2804=EDGE_CURVE('',#2316,#2314,#1386,.T.);
#2805=EDGE_CURVE('',#2313,#2315,#1387,.T.);
#2806=EDGE_CURVE('',#2317,#2318,#1388,.T.);
#2807=EDGE_CURVE('',#2318,#2316,#323,.T.);
#2808=EDGE_CURVE('',#2315,#2317,#324,.T.);
#2809=EDGE_CURVE('',#2319,#2320,#1389,.T.);
#2810=EDGE_CURVE('',#2320,#2318,#1390,.T.);
#2811=EDGE_CURVE('',#2317,#2319,#1391,.T.);
#2812=EDGE_CURVE('',#2321,#2322,#1392,.T.);
#2813=EDGE_CURVE('',#2322,#2320,#325,.T.);
#2814=EDGE_CURVE('',#2319,#2321,#326,.T.);
#2815=EDGE_CURVE('',#2323,#2324,#1393,.T.);
#2816=EDGE_CURVE('',#2324,#2322,#1394,.T.);
#2817=EDGE_CURVE('',#2321,#2323,#1395,.T.);
#2818=EDGE_CURVE('',#2323,#2325,#327,.T.);
#2819=EDGE_CURVE('',#2325,#2326,#1396,.T.);
#2820=EDGE_CURVE('',#2326,#2324,#328,.T.);
#2821=EDGE_CURVE('',#2325,#2327,#1397,.T.);
#2822=EDGE_CURVE('',#2327,#2328,#1398,.T.);
#2823=EDGE_CURVE('',#2328,#2326,#1399,.T.);
#2824=EDGE_CURVE('',#2327,#2329,#329,.T.);
#2825=EDGE_CURVE('',#2329,#2330,#1400,.T.);
#2826=EDGE_CURVE('',#2330,#2328,#330,.T.);
#2827=EDGE_CURVE('',#2329,#2331,#1401,.T.);
#2828=EDGE_CURVE('',#2331,#2332,#1402,.T.);
#2829=EDGE_CURVE('',#2332,#2330,#1403,.T.);
#2830=EDGE_CURVE('',#2331,#2333,#331,.T.);
#2831=EDGE_CURVE('',#2333,#2334,#1404,.T.);
#2832=EDGE_CURVE('',#2334,#2332,#332,.T.);
#2833=EDGE_CURVE('',#2333,#2335,#1405,.T.);
#2834=EDGE_CURVE('',#2335,#2336,#1406,.T.);
#2835=EDGE_CURVE('',#2336,#2334,#1407,.T.);
#2836=EDGE_CURVE('',#2335,#2337,#333,.T.);
#2837=EDGE_CURVE('',#2337,#2338,#1408,.T.);
#2838=EDGE_CURVE('',#2338,#2336,#334,.T.);
#2839=EDGE_CURVE('',#2337,#2339,#1409,.T.);
#2840=EDGE_CURVE('',#2339,#2340,#1410,.T.);
#2841=EDGE_CURVE('',#2340,#2338,#1411,.T.);
#2842=EDGE_CURVE('',#2339,#2341,#335,.T.);
#2843=EDGE_CURVE('',#2341,#2342,#1412,.T.);
#2844=EDGE_CURVE('',#2342,#2340,#336,.T.);
#2845=EDGE_CURVE('',#2341,#2343,#1413,.T.);
#2846=EDGE_CURVE('',#2343,#2344,#1414,.T.);
#2847=EDGE_CURVE('',#2344,#2342,#1415,.T.);
#2848=EDGE_CURVE('',#2343,#2345,#337,.T.);
#2849=EDGE_CURVE('',#2345,#2346,#1416,.T.);
#2850=EDGE_CURVE('',#2346,#2344,#338,.T.);
#2851=EDGE_CURVE('',#2345,#2347,#1417,.T.);
#2852=EDGE_CURVE('',#2347,#2348,#1418,.T.);
#2853=EDGE_CURVE('',#2348,#2346,#1419,.T.);
#2854=EDGE_CURVE('',#2347,#2349,#339,.T.);
#2855=EDGE_CURVE('',#2349,#2350,#1420,.T.);
#2856=EDGE_CURVE('',#2350,#2348,#340,.T.);
#2857=EDGE_CURVE('',#2349,#2351,#1421,.T.);
#2858=EDGE_CURVE('',#2351,#2352,#1422,.T.);
#2859=EDGE_CURVE('',#2352,#2350,#1423,.T.);
#2860=EDGE_CURVE('',#2351,#2353,#341,.T.);
#2861=EDGE_CURVE('',#2353,#2354,#1424,.T.);
#2862=EDGE_CURVE('',#2354,#2352,#342,.T.);
#2863=EDGE_CURVE('',#2353,#2355,#1425,.T.);
#2864=EDGE_CURVE('',#2355,#2356,#1426,.T.);
#2865=EDGE_CURVE('',#2356,#2354,#1427,.T.);
#2866=EDGE_CURVE('',#2357,#2358,#1428,.T.);
#2867=EDGE_CURVE('',#2358,#2356,#343,.T.);
#2868=EDGE_CURVE('',#2355,#2357,#344,.T.);
#2869=EDGE_CURVE('',#2289,#2358,#345,.T.);
#2870=EDGE_CURVE('',#2357,#2290,#346,.T.);
#2871=EDGE_CURVE('',#2359,#2328,#1429,.T.);
#2872=EDGE_CURVE('',#2360,#2359,#1430,.T.);
#2873=EDGE_CURVE('',#2360,#2326,#1431,.T.);
#2874=EDGE_CURVE('',#2361,#2330,#1432,.T.);
#2875=EDGE_CURVE('',#2359,#2361,#347,.T.);
#2876=EDGE_CURVE('',#2362,#2332,#1433,.T.);
#2877=EDGE_CURVE('',#2361,#2362,#1434,.T.);
#2878=EDGE_CURVE('',#2363,#2334,#1435,.T.);
#2879=EDGE_CURVE('',#2362,#2363,#348,.T.);
#2880=EDGE_CURVE('',#2364,#2336,#1436,.T.);
#2881=EDGE_CURVE('',#2363,#2364,#1437,.T.);
#2882=EDGE_CURVE('',#2365,#2338,#1438,.T.);
#2883=EDGE_CURVE('',#2364,#2365,#349,.T.);
#2884=EDGE_CURVE('',#2366,#2340,#1439,.T.);
#2885=EDGE_CURVE('',#2365,#2366,#1440,.T.);
#2886=EDGE_CURVE('',#2367,#2342,#1441,.T.);
#2887=EDGE_CURVE('',#2366,#2367,#350,.T.);
#2888=EDGE_CURVE('',#2368,#2344,#1442,.T.);
#2889=EDGE_CURVE('',#2367,#2368,#1443,.T.);
#2890=EDGE_CURVE('',#2369,#2346,#1444,.T.);
#2891=EDGE_CURVE('',#2368,#2369,#351,.T.);
#2892=EDGE_CURVE('',#2370,#2348,#1445,.T.);
#2893=EDGE_CURVE('',#2369,#2370,#1446,.T.);
#2894=EDGE_CURVE('',#2371,#2350,#1447,.T.);
#2895=EDGE_CURVE('',#2370,#2371,#352,.T.);
#2896=EDGE_CURVE('',#2372,#2352,#1448,.T.);
#2897=EDGE_CURVE('',#2371,#2372,#1449,.T.);
#2898=EDGE_CURVE('',#2373,#2354,#1450,.T.);
#2899=EDGE_CURVE('',#2372,#2373,#353,.T.);
#2900=EDGE_CURVE('',#2374,#2356,#1451,.T.);
#2901=EDGE_CURVE('',#2373,#2374,#1452,.T.);
#2902=EDGE_CURVE('',#2358,#2375,#1453,.T.);
#2903=EDGE_CURVE('',#2374,#2375,#354,.T.);
#2904=EDGE_CURVE('',#2376,#2289,#1454,.T.);
#2905=EDGE_CURVE('',#2375,#2376,#355,.T.);
#2906=EDGE_CURVE('',#2377,#2292,#1455,.T.);
#2907=EDGE_CURVE('',#2376,#2377,#356,.T.);
#2908=EDGE_CURVE('',#2378,#2378,#357,.T.);
#2909=EDGE_CURVE('',#2379,#2379,#358,.T.);
#2910=EDGE_CURVE('',#2380,#2380,#359,.T.);
#2911=EDGE_CURVE('',#2381,#2381,#360,.T.);
#2912=EDGE_CURVE('',#2382,#2382,#361,.T.);
#2913=EDGE_CURVE('',#2376,#2383,#174,.T.);
#2914=EDGE_CURVE('',#2383,#2384,#362,.T.);
#2915=EDGE_CURVE('',#2384,#2375,#1456,.T.);
#2916=EDGE_CURVE('',#2385,#2374,#1457,.T.);
#2917=EDGE_CURVE('',#2384,#2385,#363,.T.);
#2918=EDGE_CURVE('',#2386,#2373,#1458,.T.);
#2919=EDGE_CURVE('',#2385,#2386,#1459,.T.);
#2920=EDGE_CURVE('',#2387,#2372,#1460,.T.);
#2921=EDGE_CURVE('',#2386,#2387,#364,.T.);
#2922=EDGE_CURVE('',#2387,#2388,#1461,.T.);
#2923=EDGE_CURVE('',#2388,#2371,#1462,.T.);
#2924=EDGE_CURVE('',#2389,#2370,#1463,.T.);
#2925=EDGE_CURVE('',#2388,#2389,#365,.T.);
#2926=EDGE_CURVE('',#2389,#2390,#1464,.T.);
#2927=EDGE_CURVE('',#2390,#2369,#1465,.T.);
#2928=EDGE_CURVE('',#2391,#2368,#1466,.T.);
#2929=EDGE_CURVE('',#2390,#2391,#366,.T.);
#2930=EDGE_CURVE('',#2391,#2392,#1467,.T.);
#2931=EDGE_CURVE('',#2392,#2367,#1468,.T.);
#2932=EDGE_CURVE('',#2393,#2366,#1469,.T.);
#2933=EDGE_CURVE('',#2392,#2393,#367,.T.);
#2934=EDGE_CURVE('',#2393,#2394,#1470,.T.);
#2935=EDGE_CURVE('',#2394,#2365,#1471,.T.);
#2936=EDGE_CURVE('',#2395,#2364,#1472,.T.);
#2937=EDGE_CURVE('',#2394,#2395,#368,.T.);
#2938=EDGE_CURVE('',#2395,#2396,#1473,.T.);
#2939=EDGE_CURVE('',#2396,#2363,#1474,.T.);
#2940=EDGE_CURVE('',#2397,#2362,#1475,.T.);
#2941=EDGE_CURVE('',#2396,#2397,#369,.T.);
#2942=EDGE_CURVE('',#2398,#2361,#1476,.T.);
#2943=EDGE_CURVE('',#2397,#2398,#1477,.T.);
#2944=EDGE_CURVE('',#2399,#2359,#1478,.T.);
#2945=EDGE_CURVE('',#2398,#2399,#370,.T.);
#2946=EDGE_CURVE('',#2400,#2360,#1479,.T.);
#2947=EDGE_CURVE('',#2399,#2400,#1480,.T.);
#2948=EDGE_CURVE('',#2401,#2402,#1481,.T.);
#2949=EDGE_CURVE('',#2402,#2360,#371,.T.);
#2950=EDGE_CURVE('',#2400,#2401,#372,.T.);
#2951=EDGE_CURVE('',#2401,#2403,#1482,.T.);
#2952=EDGE_CURVE('',#2403,#2404,#1483,.T.);
#2953=EDGE_CURVE('',#2404,#2402,#1484,.T.);
#2954=EDGE_CURVE('',#2403,#2405,#373,.T.);
#2955=EDGE_CURVE('',#2405,#2406,#1485,.T.);
#2956=EDGE_CURVE('',#2406,#2404,#374,.T.);
#2957=EDGE_CURVE('',#2405,#2407,#1486,.T.);
#2958=EDGE_CURVE('',#2407,#2408,#1487,.T.);
#2959=EDGE_CURVE('',#2408,#2406,#1488,.T.);
#2960=EDGE_CURVE('',#2407,#2409,#375,.T.);
#2961=EDGE_CURVE('',#2409,#2410,#1489,.T.);
#2962=EDGE_CURVE('',#2410,#2408,#376,.T.);
#2963=EDGE_CURVE('',#2411,#2412,#1490,.T.);
#2964=EDGE_CURVE('',#2412,#2410,#1491,.T.);
#2965=EDGE_CURVE('',#2409,#2411,#1492,.T.);
#2966=EDGE_CURVE('',#2411,#2413,#377,.T.);
#2967=EDGE_CURVE('',#2413,#2414,#1493,.T.);
#2968=EDGE_CURVE('',#2414,#2412,#378,.T.);
#2969=EDGE_CURVE('',#2415,#2416,#1494,.T.);
#2970=EDGE_CURVE('',#2416,#2414,#1495,.T.);
#2971=EDGE_CURVE('',#2413,#2415,#1496,.T.);
#2972=EDGE_CURVE('',#2415,#2417,#379,.T.);
#2973=EDGE_CURVE('',#2417,#2418,#1497,.T.);
#2974=EDGE_CURVE('',#2418,#2416,#380,.T.);
#2975=EDGE_CURVE('',#2419,#2420,#1498,.T.);
#2976=EDGE_CURVE('',#2420,#2418,#1499,.T.);
#2977=EDGE_CURVE('',#2417,#2419,#1500,.T.);
#2978=EDGE_CURVE('',#2419,#2421,#381,.T.);
#2979=EDGE_CURVE('',#2421,#2422,#1501,.T.);
#2980=EDGE_CURVE('',#2422,#2420,#382,.T.);
#2981=EDGE_CURVE('',#2423,#2424,#1502,.T.);
#2982=EDGE_CURVE('',#2424,#2422,#1503,.T.);
#2983=EDGE_CURVE('',#2421,#2423,#1504,.T.);
#2984=EDGE_CURVE('',#2423,#2425,#383,.T.);
#2985=EDGE_CURVE('',#2425,#2426,#1505,.T.);
#2986=EDGE_CURVE('',#2426,#2424,#384,.T.);
#2987=EDGE_CURVE('',#2427,#2428,#1506,.T.);
#2988=EDGE_CURVE('',#2428,#2426,#1507,.T.);
#2989=EDGE_CURVE('',#2425,#2427,#1508,.T.);
#2990=EDGE_CURVE('',#2427,#2429,#385,.T.);
#2991=EDGE_CURVE('',#2429,#2430,#1509,.T.);
#2992=EDGE_CURVE('',#2430,#2428,#386,.T.);
#2993=EDGE_CURVE('',#2429,#2431,#1510,.T.);
#2994=EDGE_CURVE('',#2431,#2432,#1511,.T.);
#2995=EDGE_CURVE('',#2432,#2430,#1512,.T.);
#2996=EDGE_CURVE('',#2433,#2377,#1513,.T.);
#2997=EDGE_CURVE('',#2377,#2432,#387,.T.);
#2998=EDGE_CURVE('',#2431,#2433,#388,.T.);
#2999=EDGE_CURVE('',#2433,#2383,#389,.T.);
#3000=EDGE_CURVE('',#2402,#2324,#1514,.T.);
#3001=EDGE_CURVE('',#2404,#2322,#1515,.T.);
#3002=EDGE_CURVE('',#2406,#2320,#1516,.T.);
#3003=EDGE_CURVE('',#2408,#2318,#1517,.T.);
#3004=EDGE_CURVE('',#2410,#2316,#1518,.T.);
#3005=EDGE_CURVE('',#2412,#2314,#1519,.T.);
#3006=EDGE_CURVE('',#2414,#2312,#1520,.T.);
#3007=EDGE_CURVE('',#2416,#2310,#1521,.T.);
#3008=EDGE_CURVE('',#2418,#2308,#1522,.T.);
#3009=EDGE_CURVE('',#2420,#2306,#1523,.T.);
#3010=EDGE_CURVE('',#2422,#2304,#1524,.T.);
#3011=EDGE_CURVE('',#2424,#2302,#1525,.T.);
#3012=EDGE_CURVE('',#2426,#2300,#1526,.T.);
#3013=EDGE_CURVE('',#2428,#2298,#1527,.T.);
#3014=EDGE_CURVE('',#2430,#2296,#1528,.T.);
#3015=EDGE_CURVE('',#2294,#2432,#1529,.T.);
#3016=EDGE_CURVE('',#2434,#2434,#390,.T.);
#3017=EDGE_CURVE('',#2435,#2435,#391,.T.);
#3018=EDGE_CURVE('',#2436,#2436,#392,.T.);
#3019=EDGE_CURVE('',#2437,#2437,#393,.T.);
#3020=EDGE_CURVE('',#2438,#2438,#394,.T.);
#3021=EDGE_CURVE('',#2439,#2439,#395,.T.);
#3022=EDGE_CURVE('',#2439,#2378,#1530,.T.);
#3023=EDGE_CURVE('',#2439,#2435,#1531,.T.);
#3024=EDGE_CURVE('',#2440,#2440,#396,.T.);
#3025=EDGE_CURVE('',#2440,#2382,#1532,.T.);
#3026=EDGE_CURVE('',#2440,#2436,#1533,.T.);
#3027=EDGE_CURVE('',#2379,#2441,#1534,.T.);
#3028=EDGE_CURVE('',#2441,#2441,#397,.T.);
#3029=EDGE_CURVE('',#2441,#2434,#1535,.T.);
#3030=EDGE_CURVE('',#2380,#2437,#1536,.T.);
#3031=EDGE_CURVE('',#2381,#2438,#1537,.T.);
#3032=EDGE_CURVE('',#2442,#2442,#398,.T.);
#3033=EDGE_CURVE('',#2442,#2443,#1538,.T.);
#3034=EDGE_CURVE('',#2443,#2443,#399,.T.);
#3035=EDGE_CURVE('',#2443,#2444,#1539,.T.);
#3036=EDGE_CURVE('',#2444,#2444,#400,.T.);
#3037=EDGE_CURVE('',#2444,#2445,#1540,.T.);
#3038=EDGE_CURVE('',#2445,#2445,#401,.T.);
#3039=EDGE_CURVE('',#2446,#2446,#402,.T.);
#3040=EDGE_CURVE('',#2446,#2446,#403,.T.);
#3041=EDGE_CURVE('',#2447,#2448,#404,.T.);
#3042=EDGE_CURVE('',#2447,#2448,#175,.T.);
#3043=EDGE_CURVE('',#2448,#2449,#176,.T.);
#3044=EDGE_CURVE('',#2449,#2449,#405,.T.);
#3045=EDGE_CURVE('',#2450,#2450,#406,.T.);
#3046=EDGE_CURVE('',#2451,#2450,#407,.T.);
#3047=EDGE_CURVE('',#2452,#2452,#408,.T.);
#3048=EDGE_CURVE('',#2452,#2453,#409,.T.);
#3049=EDGE_CURVE('',#2453,#2453,#410,.T.);
#3050=EDGE_CURVE('',#2453,#2454,#1541,.T.);
#3051=EDGE_CURVE('',#2454,#2454,#411,.T.);
#3052=EDGE_CURVE('',#2455,#2456,#1542,.T.);
#3053=EDGE_CURVE('',#2455,#2457,#1543,.T.);
#3054=EDGE_CURVE('',#2457,#2458,#1544,.T.);
#3055=EDGE_CURVE('',#2456,#2458,#1545,.T.);
#3056=EDGE_CURVE('',#2459,#2455,#1546,.T.);
#3057=EDGE_CURVE('',#2459,#2460,#1547,.T.);
#3058=EDGE_CURVE('',#2460,#2457,#1548,.T.);
#3059=EDGE_CURVE('',#2461,#2459,#1549,.T.);
#3060=EDGE_CURVE('',#2461,#2462,#1550,.T.);
#3061=EDGE_CURVE('',#2462,#2460,#1551,.T.);
#3062=EDGE_CURVE('',#2463,#2461,#1552,.T.);
#3063=EDGE_CURVE('',#2463,#2464,#1553,.T.);
#3064=EDGE_CURVE('',#2464,#2462,#1554,.T.);
#3065=EDGE_CURVE('',#2465,#2463,#1555,.T.);
#3066=EDGE_CURVE('',#2465,#2466,#1556,.T.);
#3067=EDGE_CURVE('',#2466,#2464,#1557,.T.);
#3068=EDGE_CURVE('',#2456,#2465,#1558,.T.);
#3069=EDGE_CURVE('',#2458,#2466,#1559,.T.);
#3070=EDGE_CURVE('',#2467,#2467,#412,.T.);
#3071=EDGE_CURVE('',#2467,#2454,#1560,.T.);
#3072=EDGE_CURVE('',#2468,#2468,#413,.T.);
#3073=EDGE_CURVE('',#2468,#2469,#414,.T.);
#3074=EDGE_CURVE('',#2470,#2471,#1561,.T.);
#3075=EDGE_CURVE('',#2472,#2470,#415,.T.);
#3076=EDGE_CURVE('',#2473,#2472,#1562,.T.);
#3077=EDGE_CURVE('',#2474,#2473,#416,.T.);
#3078=EDGE_CURVE('',#2475,#2474,#1563,.T.);
#3079=EDGE_CURVE('',#2476,#2475,#417,.T.);
#3080=EDGE_CURVE('',#2477,#2476,#1564,.T.);
#3081=EDGE_CURVE('',#2478,#2477,#418,.T.);
#3082=EDGE_CURVE('',#2479,#2478,#1565,.T.);
#3083=EDGE_CURVE('',#2480,#2479,#419,.T.);
#3084=EDGE_CURVE('',#2481,#2480,#1566,.T.);
#3085=EDGE_CURVE('',#2482,#2481,#420,.T.);
#3086=EDGE_CURVE('',#2483,#2482,#1567,.T.);
#3087=EDGE_CURVE('',#2484,#2483,#421,.T.);
#3088=EDGE_CURVE('',#2485,#2484,#422,.T.);
#3089=EDGE_CURVE('',#2486,#2485,#1568,.T.);
#3090=EDGE_CURVE('',#2487,#2486,#423,.T.);
#3091=EDGE_CURVE('',#2488,#2487,#1569,.T.);
#3092=EDGE_CURVE('',#2489,#2488,#424,.T.);
#3093=EDGE_CURVE('',#2490,#2489,#1570,.T.);
#3094=EDGE_CURVE('',#2491,#2490,#425,.T.);
#3095=EDGE_CURVE('',#2492,#2491,#426,.T.);
#3096=EDGE_CURVE('',#2493,#2492,#1571,.T.);
#3097=EDGE_CURVE('',#2494,#2493,#427,.T.);
#3098=EDGE_CURVE('',#2495,#2494,#1572,.T.);
#3099=EDGE_CURVE('',#2496,#2495,#428,.T.);
#3100=EDGE_CURVE('',#2497,#2496,#1573,.T.);
#3101=EDGE_CURVE('',#2471,#2497,#429,.T.);
#3102=EDGE_CURVE('',#2498,#2498,#430,.T.);
#3103=EDGE_CURVE('',#2499,#2499,#431,.T.);
#3104=EDGE_CURVE('',#2500,#2500,#432,.T.);
#3105=EDGE_CURVE('',#2501,#2501,#433,.T.);
#3106=EDGE_CURVE('',#2502,#2502,#434,.T.);
#3107=EDGE_CURVE('',#2503,#2503,#435,.T.);
#3108=EDGE_CURVE('',#2504,#2504,#436,.T.);
#3109=EDGE_CURVE('',#2504,#2505,#437,.T.);
#3110=EDGE_CURVE('',#2503,#2506,#438,.T.);
#3111=EDGE_CURVE('',#2502,#2507,#1574,.T.);
#3112=EDGE_CURVE('',#2507,#2507,#439,.T.);
#3113=EDGE_CURVE('',#2508,#2508,#440,.T.);
#3114=EDGE_CURVE('',#2508,#2507,#1575,.T.);
#3115=EDGE_CURVE('',#2498,#2509,#1576,.T.);
#3116=EDGE_CURVE('',#2509,#2509,#441,.T.);
#3117=EDGE_CURVE('',#2510,#2510,#442,.T.);
#3118=EDGE_CURVE('',#2510,#2509,#1577,.T.);
#3119=EDGE_CURVE('',#2511,#2511,#443,.T.);
#3120=EDGE_CURVE('',#2511,#2501,#1578,.T.);
#3121=EDGE_CURVE('',#2512,#2512,#444,.T.);
#3122=EDGE_CURVE('',#2512,#2511,#1579,.T.);
#3123=EDGE_CURVE('',#2513,#2513,#445,.T.);
#3124=EDGE_CURVE('',#2513,#2499,#1580,.T.);
#3125=EDGE_CURVE('',#2514,#2514,#446,.T.);
#3126=EDGE_CURVE('',#2514,#2513,#1581,.T.);
#3127=EDGE_CURVE('',#2508,#2515,#1582,.T.);
#3128=EDGE_CURVE('',#2515,#2515,#447,.T.);
#3129=EDGE_CURVE('',#2516,#2517,#1583,.T.);
#3130=EDGE_CURVE('',#2518,#2516,#448,.T.);
#3131=EDGE_CURVE('',#2519,#2518,#1584,.T.);
#3132=EDGE_CURVE('',#2520,#2519,#449,.T.);
#3133=EDGE_CURVE('',#2521,#2520,#1585,.T.);
#3134=EDGE_CURVE('',#2522,#2521,#450,.T.);
#3135=EDGE_CURVE('',#2523,#2522,#1586,.T.);
#3136=EDGE_CURVE('',#2524,#2523,#451,.T.);
#3137=EDGE_CURVE('',#2525,#2524,#452,.T.);
#3138=EDGE_CURVE('',#2526,#2525,#1587,.T.);
#3139=EDGE_CURVE('',#2527,#2526,#453,.T.);
#3140=EDGE_CURVE('',#2528,#2527,#1588,.T.);
#3141=EDGE_CURVE('',#2529,#2528,#454,.T.);
#3142=EDGE_CURVE('',#2530,#2529,#1589,.T.);
#3143=EDGE_CURVE('',#2531,#2530,#455,.T.);
#3144=EDGE_CURVE('',#2532,#2531,#456,.T.);
#3145=EDGE_CURVE('',#2533,#2532,#1590,.T.);
#3146=EDGE_CURVE('',#2534,#2533,#457,.T.);
#3147=EDGE_CURVE('',#2535,#2534,#1591,.T.);
#3148=EDGE_CURVE('',#2536,#2535,#458,.T.);
#3149=EDGE_CURVE('',#2537,#2536,#1592,.T.);
#3150=EDGE_CURVE('',#2538,#2537,#459,.T.);
#3151=EDGE_CURVE('',#2539,#2538,#1593,.T.);
#3152=EDGE_CURVE('',#2540,#2539,#460,.T.);
#3153=EDGE_CURVE('',#2541,#2540,#1594,.T.);
#3154=EDGE_CURVE('',#2542,#2541,#461,.T.);
#3155=EDGE_CURVE('',#2543,#2542,#1595,.T.);
#3156=EDGE_CURVE('',#2517,#2543,#462,.T.);
#3157=EDGE_CURVE('',#2544,#2544,#463,.T.);
#3158=EDGE_CURVE('',#2545,#2545,#464,.T.);
#3159=EDGE_CURVE('',#2546,#2546,#465,.T.);
#3160=EDGE_CURVE('',#2547,#2547,#466,.T.);
#3161=EDGE_CURVE('',#2510,#2544,#1596,.T.);
#3162=EDGE_CURVE('',#2547,#2512,#1597,.T.);
#3163=EDGE_CURVE('',#2545,#2514,#1598,.T.);
#3164=EDGE_CURVE('',#2548,#2516,#1599,.T.);
#3165=EDGE_CURVE('',#2517,#2549,#1600,.T.);
#3166=EDGE_CURVE('',#2549,#2548,#1601,.T.);
#3167=EDGE_CURVE('',#2548,#2550,#467,.T.);
#3168=EDGE_CURVE('',#2550,#2518,#1602,.T.);
#3169=EDGE_CURVE('',#2551,#2519,#1603,.T.);
#3170=EDGE_CURVE('',#2550,#2551,#1604,.T.);
#3171=EDGE_CURVE('',#2551,#2552,#468,.T.);
#3172=EDGE_CURVE('',#2552,#2520,#1605,.T.);
#3173=EDGE_CURVE('',#2553,#2521,#1606,.T.);
#3174=EDGE_CURVE('',#2552,#2553,#1607,.T.);
#3175=EDGE_CURVE('',#2553,#2554,#469,.T.);
#3176=EDGE_CURVE('',#2554,#2522,#1608,.T.);
#3177=EDGE_CURVE('',#2555,#2523,#1609,.T.);
#3178=EDGE_CURVE('',#2554,#2555,#1610,.T.);
#3179=EDGE_CURVE('',#2556,#2524,#1611,.T.);
#3180=EDGE_CURVE('',#2555,#2556,#470,.T.);
#3181=EDGE_CURVE('',#2556,#2557,#471,.T.);
#3182=EDGE_CURVE('',#2557,#2525,#1612,.T.);
#3183=EDGE_CURVE('',#2558,#2526,#1613,.T.);
#3184=EDGE_CURVE('',#2557,#2558,#1614,.T.);
#3185=EDGE_CURVE('',#2558,#2559,#472,.T.);
#3186=EDGE_CURVE('',#2559,#2527,#1615,.T.);
#3187=EDGE_CURVE('',#2560,#2528,#1616,.T.);
#3188=EDGE_CURVE('',#2559,#2560,#1617,.T.);
#3189=EDGE_CURVE('',#2560,#2561,#473,.T.);
#3190=EDGE_CURVE('',#2561,#2529,#1618,.T.);
#3191=EDGE_CURVE('',#2561,#2562,#1619,.T.);
#3192=EDGE_CURVE('',#2562,#2530,#1620,.T.);
#3193=EDGE_CURVE('',#2562,#2563,#474,.T.);
#3194=EDGE_CURVE('',#2563,#2531,#1621,.T.);
#3195=EDGE_CURVE('',#2563,#2564,#475,.T.);
#3196=EDGE_CURVE('',#2564,#2532,#1622,.T.);
#3197=EDGE_CURVE('',#2564,#2565,#1623,.T.);
#3198=EDGE_CURVE('',#2565,#2533,#1624,.T.);
#3199=EDGE_CURVE('',#2565,#2566,#476,.T.);
#3200=EDGE_CURVE('',#2566,#2534,#1625,.T.);
#3201=EDGE_CURVE('',#2566,#2567,#1626,.T.);
#3202=EDGE_CURVE('',#2567,#2535,#1627,.T.);
#3203=EDGE_CURVE('',#2567,#2568,#477,.T.);
#3204=EDGE_CURVE('',#2568,#2536,#1628,.T.);
#3205=EDGE_CURVE('',#2568,#2569,#1629,.T.);
#3206=EDGE_CURVE('',#2569,#2537,#1630,.T.);
#3207=EDGE_CURVE('',#2569,#2570,#478,.T.);
#3208=EDGE_CURVE('',#2570,#2538,#1631,.T.);
#3209=EDGE_CURVE('',#2570,#2571,#1632,.T.);
#3210=EDGE_CURVE('',#2571,#2539,#1633,.T.);
#3211=EDGE_CURVE('',#2571,#2572,#479,.T.);
#3212=EDGE_CURVE('',#2572,#2540,#1634,.T.);
#3213=EDGE_CURVE('',#2572,#2573,#1635,.T.);
#3214=EDGE_CURVE('',#2573,#2541,#1636,.T.);
#3215=EDGE_CURVE('',#2573,#2574,#480,.T.);
#3216=EDGE_CURVE('',#2574,#2542,#1637,.T.);
#3217=EDGE_CURVE('',#2575,#2543,#1638,.T.);
#3218=EDGE_CURVE('',#2574,#2575,#1639,.T.);
#3219=EDGE_CURVE('',#2575,#2549,#481,.T.);
#3220=EDGE_CURVE('',#2576,#2561,#1640,.T.);
#3221=EDGE_CURVE('',#2577,#2576,#1641,.T.);
#3222=EDGE_CURVE('',#2562,#2577,#1642,.T.);
#3223=EDGE_CURVE('',#2560,#2578,#1643,.T.);
#3224=EDGE_CURVE('',#2576,#2578,#482,.T.);
#3225=EDGE_CURVE('',#2579,#2559,#1644,.T.);
#3226=EDGE_CURVE('',#2578,#2579,#1645,.T.);
#3227=EDGE_CURVE('',#2558,#2580,#1646,.T.);
#3228=EDGE_CURVE('',#2579,#2580,#483,.T.);
#3229=EDGE_CURVE('',#2581,#2557,#1647,.T.);
#3230=EDGE_CURVE('',#2580,#2581,#1648,.T.);
#3231=EDGE_CURVE('',#2556,#2582,#1649,.T.);
#3232=EDGE_CURVE('',#2581,#2582,#484,.T.);
#3233=EDGE_CURVE('',#2583,#2555,#1650,.T.);
#3234=EDGE_CURVE('',#2582,#2583,#485,.T.);
#3235=EDGE_CURVE('',#2584,#2554,#1651,.T.);
#3236=EDGE_CURVE('',#2583,#2584,#1652,.T.);
#3237=EDGE_CURVE('',#2553,#2585,#1653,.T.);
#3238=EDGE_CURVE('',#2584,#2585,#486,.T.);
#3239=EDGE_CURVE('',#2586,#2552,#1654,.T.);
#3240=EDGE_CURVE('',#2585,#2586,#1655,.T.);
#3241=EDGE_CURVE('',#2551,#2587,#1656,.T.);
#3242=EDGE_CURVE('',#2586,#2587,#487,.T.);
#3243=EDGE_CURVE('',#2588,#2550,#1657,.T.);
#3244=EDGE_CURVE('',#2587,#2588,#1658,.T.);
#3245=EDGE_CURVE('',#2548,#2589,#1659,.T.);
#3246=EDGE_CURVE('',#2588,#2589,#488,.T.);
#3247=EDGE_CURVE('',#2590,#2549,#1660,.T.);
#3248=EDGE_CURVE('',#2589,#2590,#1661,.T.);
#3249=EDGE_CURVE('',#2471,#2589,#1662,.T.);
#3250=EDGE_CURVE('',#2590,#2470,#1663,.T.);
#3251=EDGE_CURVE('',#2497,#2588,#1664,.T.);
#3252=EDGE_CURVE('',#2496,#2587,#1665,.T.);
#3253=EDGE_CURVE('',#2495,#2586,#1666,.T.);
#3254=EDGE_CURVE('',#2494,#2585,#1667,.T.);
#3255=EDGE_CURVE('',#2493,#2584,#1668,.T.);
#3256=EDGE_CURVE('',#2492,#2583,#1669,.T.);
#3257=EDGE_CURVE('',#2491,#2582,#1670,.T.);
#3258=EDGE_CURVE('',#2490,#2581,#1671,.T.);
#3259=EDGE_CURVE('',#2489,#2580,#1672,.T.);
#3260=EDGE_CURVE('',#2488,#2579,#1673,.T.);
#3261=EDGE_CURVE('',#2487,#2578,#1674,.T.);
#3262=EDGE_CURVE('',#2486,#2576,#1675,.T.);
#3263=EDGE_CURVE('',#2485,#2577,#1676,.T.);
#3264=EDGE_CURVE('',#2484,#2591,#1677,.T.);
#3265=EDGE_CURVE('',#2591,#2577,#489,.T.);
#3266=EDGE_CURVE('',#2483,#2592,#1678,.T.);
#3267=EDGE_CURVE('',#2592,#2591,#490,.T.);
#3268=EDGE_CURVE('',#2482,#2593,#1679,.T.);
#3269=EDGE_CURVE('',#2593,#2592,#1680,.T.);
#3270=EDGE_CURVE('',#2481,#2594,#1681,.T.);
#3271=EDGE_CURVE('',#2594,#2593,#491,.T.);
#3272=EDGE_CURVE('',#2480,#2595,#1682,.T.);
#3273=EDGE_CURVE('',#2595,#2594,#1683,.T.);
#3274=EDGE_CURVE('',#2479,#2596,#1684,.T.);
#3275=EDGE_CURVE('',#2596,#2595,#492,.T.);
#3276=EDGE_CURVE('',#2478,#2597,#1685,.T.);
#3277=EDGE_CURVE('',#2597,#2596,#1686,.T.);
#3278=EDGE_CURVE('',#2477,#2598,#1687,.T.);
#3279=EDGE_CURVE('',#2598,#2597,#493,.T.);
#3280=EDGE_CURVE('',#2476,#2599,#1688,.T.);
#3281=EDGE_CURVE('',#2599,#2598,#1689,.T.);
#3282=EDGE_CURVE('',#2475,#2600,#1690,.T.);
#3283=EDGE_CURVE('',#2600,#2599,#494,.T.);
#3284=EDGE_CURVE('',#2474,#2601,#1691,.T.);
#3285=EDGE_CURVE('',#2601,#2600,#1692,.T.);
#3286=EDGE_CURVE('',#2473,#2602,#1693,.T.);
#3287=EDGE_CURVE('',#2602,#2601,#495,.T.);
#3288=EDGE_CURVE('',#2472,#2603,#1694,.T.);
#3289=EDGE_CURVE('',#2603,#2602,#1695,.T.);
#3290=EDGE_CURVE('',#2590,#2603,#496,.T.);
#3291=EDGE_CURVE('',#2591,#2563,#1696,.T.);
#3292=EDGE_CURVE('',#2592,#2564,#1697,.T.);
#3293=EDGE_CURVE('',#2565,#2593,#1698,.T.);
#3294=EDGE_CURVE('',#2594,#2566,#1699,.T.);
#3295=EDGE_CURVE('',#2567,#2595,#1700,.T.);
#3296=EDGE_CURVE('',#2596,#2568,#1701,.T.);
#3297=EDGE_CURVE('',#2569,#2597,#1702,.T.);
#3298=EDGE_CURVE('',#2598,#2570,#1703,.T.);
#3299=EDGE_CURVE('',#2571,#2599,#1704,.T.);
#3300=EDGE_CURVE('',#2600,#2572,#1705,.T.);
#3301=EDGE_CURVE('',#2601,#2573,#1706,.T.);
#3302=EDGE_CURVE('',#2602,#2574,#1707,.T.);
#3303=EDGE_CURVE('',#2575,#2603,#1708,.T.);
#3304=EDGE_CURVE('',#2546,#2500,#1709,.T.);
#3305=EDGE_CURVE('',#2604,#2604,#497,.T.);
#3306=EDGE_CURVE('',#2604,#2605,#1710,.T.);
#3307=EDGE_CURVE('',#2605,#2605,#498,.T.);
#3308=EDGE_CURVE('',#2605,#2606,#1711,.T.);
#3309=EDGE_CURVE('',#2606,#2606,#499,.T.);
#3310=EDGE_CURVE('',#2606,#2607,#1712,.T.);
#3311=EDGE_CURVE('',#2607,#2607,#500,.T.);
#3312=EDGE_CURVE('',#2608,#2608,#501,.T.);
#3313=EDGE_CURVE('',#2609,#2608,#502,.T.);
#3314=EDGE_CURVE('',#2610,#2610,#503,.T.);
#3315=EDGE_CURVE('',#2610,#2611,#504,.T.);
#3316=EDGE_CURVE('',#2611,#2611,#505,.T.);
#3317=EDGE_CURVE('',#2611,#2612,#1713,.T.);
#3318=EDGE_CURVE('',#2612,#2612,#506,.T.);
#3319=EDGE_CURVE('',#2613,#2614,#1714,.T.);
#3320=EDGE_CURVE('',#2613,#2615,#1715,.T.);
#3321=EDGE_CURVE('',#2615,#2616,#1716,.T.);
#3322=EDGE_CURVE('',#2614,#2616,#1717,.T.);
#3323=EDGE_CURVE('',#2617,#2613,#1718,.T.);
#3324=EDGE_CURVE('',#2617,#2618,#1719,.T.);
#3325=EDGE_CURVE('',#2618,#2615,#1720,.T.);
#3326=EDGE_CURVE('',#2619,#2617,#1721,.T.);
#3327=EDGE_CURVE('',#2619,#2620,#1722,.T.);
#3328=EDGE_CURVE('',#2620,#2618,#1723,.T.);
#3329=EDGE_CURVE('',#2621,#2619,#1724,.T.);
#3330=EDGE_CURVE('',#2621,#2622,#1725,.T.);
#3331=EDGE_CURVE('',#2622,#2620,#1726,.T.);
#3332=EDGE_CURVE('',#2623,#2621,#1727,.T.);
#3333=EDGE_CURVE('',#2623,#2624,#1728,.T.);
#3334=EDGE_CURVE('',#2624,#2622,#1729,.T.);
#3335=EDGE_CURVE('',#2614,#2623,#1730,.T.);
#3336=EDGE_CURVE('',#2616,#2624,#1731,.T.);
#3337=EDGE_CURVE('',#2625,#2625,#507,.T.);
#3338=EDGE_CURVE('',#2625,#2612,#1732,.T.);
#3339=EDGE_CURVE('',#2626,#2626,#508,.T.);
#3340=EDGE_CURVE('',#2626,#2626,#509,.T.);
#3341=EDGE_CURVE('',#2627,#2628,#510,.T.);
#3342=EDGE_CURVE('',#2627,#2628,#177,.T.);
#3343=EDGE_CURVE('',#2628,#2629,#178,.T.);
#3344=EDGE_CURVE('',#2629,#2629,#511,.T.);
#3345=EDGE_CURVE('',#2630,#2630,#512,.T.);
#3346=EDGE_CURVE('',#2630,#2630,#513,.T.);
#3347=EDGE_CURVE('',#2631,#2632,#514,.T.);
#3348=EDGE_CURVE('',#2631,#2632,#179,.T.);
#3349=EDGE_CURVE('',#2632,#2633,#180,.T.);
#3350=EDGE_CURVE('',#2633,#2633,#515,.T.);
#3351=EDGE_CURVE('',#2634,#2634,#516,.T.);
#3352=EDGE_CURVE('',#2634,#2635,#1733,.T.);
#3353=EDGE_CURVE('',#2635,#2635,#517,.T.);
#3354=EDGE_CURVE('',#2635,#2636,#1734,.T.);
#3355=EDGE_CURVE('',#2636,#2636,#518,.T.);
#3356=EDGE_CURVE('',#2636,#2637,#1735,.T.);
#3357=EDGE_CURVE('',#2637,#2637,#519,.T.);
#3358=EDGE_CURVE('',#2638,#2638,#520,.T.);
#3359=EDGE_CURVE('',#2638,#2638,#521,.T.);
#3360=EDGE_CURVE('',#2639,#2640,#522,.T.);
#3361=EDGE_CURVE('',#2639,#2640,#181,.T.);
#3362=EDGE_CURVE('',#2640,#2641,#182,.T.);
#3363=EDGE_CURVE('',#2641,#2641,#523,.T.);
#3364=EDGE_CURVE('',#2642,#2642,#524,.T.);
#3365=EDGE_CURVE('',#2642,#2643,#1736,.T.);
#3366=EDGE_CURVE('',#2643,#2643,#525,.T.);
#3367=EDGE_CURVE('',#2643,#2644,#1737,.T.);
#3368=EDGE_CURVE('',#2644,#2644,#526,.T.);
#3369=EDGE_CURVE('',#2644,#2645,#1738,.T.);
#3370=EDGE_CURVE('',#2645,#2645,#527,.T.);
#3371=EDGE_CURVE('',#2646,#2646,#528,.T.);
#3372=EDGE_CURVE('',#2647,#2646,#529,.T.);
#3373=EDGE_CURVE('',#2648,#2648,#530,.T.);
#3374=EDGE_CURVE('',#2648,#2649,#531,.T.);
#3375=EDGE_CURVE('',#2649,#2649,#532,.T.);
#3376=EDGE_CURVE('',#2649,#2650,#1739,.T.);
#3377=EDGE_CURVE('',#2650,#2650,#533,.T.);
#3378=EDGE_CURVE('',#2651,#2652,#1740,.T.);
#3379=EDGE_CURVE('',#2651,#2653,#1741,.T.);
#3380=EDGE_CURVE('',#2653,#2654,#1742,.T.);
#3381=EDGE_CURVE('',#2652,#2654,#1743,.T.);
#3382=EDGE_CURVE('',#2655,#2651,#1744,.T.);
#3383=EDGE_CURVE('',#2655,#2656,#1745,.T.);
#3384=EDGE_CURVE('',#2656,#2653,#1746,.T.);
#3385=EDGE_CURVE('',#2657,#2655,#1747,.T.);
#3386=EDGE_CURVE('',#2657,#2658,#1748,.T.);
#3387=EDGE_CURVE('',#2658,#2656,#1749,.T.);
#3388=EDGE_CURVE('',#2659,#2657,#1750,.T.);
#3389=EDGE_CURVE('',#2659,#2660,#1751,.T.);
#3390=EDGE_CURVE('',#2660,#2658,#1752,.T.);
#3391=EDGE_CURVE('',#2661,#2659,#1753,.T.);
#3392=EDGE_CURVE('',#2661,#2662,#1754,.T.);
#3393=EDGE_CURVE('',#2662,#2660,#1755,.T.);
#3394=EDGE_CURVE('',#2652,#2661,#1756,.T.);
#3395=EDGE_CURVE('',#2654,#2662,#1757,.T.);
#3396=EDGE_CURVE('',#2663,#2663,#534,.T.);
#3397=EDGE_CURVE('',#2663,#2650,#1758,.T.);
#3398=ORIENTED_EDGE('',*,*,#2664,.F.);
#3399=ORIENTED_EDGE('',*,*,#2665,.T.);
#3400=ORIENTED_EDGE('',*,*,#2666,.T.);
#3401=ORIENTED_EDGE('',*,*,#2667,.F.);
#3402=ORIENTED_EDGE('',*,*,#2668,.F.);
#3403=ORIENTED_EDGE('',*,*,#2669,.T.);
#3404=ORIENTED_EDGE('',*,*,#2670,.T.);
#3405=ORIENTED_EDGE('',*,*,#2665,.F.);
#3406=ORIENTED_EDGE('',*,*,#2671,.F.);
#3407=ORIENTED_EDGE('',*,*,#2672,.T.);
#3408=ORIENTED_EDGE('',*,*,#2673,.T.);
#3409=ORIENTED_EDGE('',*,*,#2669,.F.);
#3410=ORIENTED_EDGE('',*,*,#2674,.F.);
#3411=ORIENTED_EDGE('',*,*,#2675,.T.);
#3412=ORIENTED_EDGE('',*,*,#2676,.T.);
#3413=ORIENTED_EDGE('',*,*,#2672,.F.);
#3414=ORIENTED_EDGE('',*,*,#2677,.F.);
#3415=ORIENTED_EDGE('',*,*,#2678,.T.);
#3416=ORIENTED_EDGE('',*,*,#2679,.T.);
#3417=ORIENTED_EDGE('',*,*,#2675,.F.);
#3418=ORIENTED_EDGE('',*,*,#2680,.F.);
#3419=ORIENTED_EDGE('',*,*,#2681,.T.);
#3420=ORIENTED_EDGE('',*,*,#2682,.T.);
#3421=ORIENTED_EDGE('',*,*,#2678,.F.);
#3422=ORIENTED_EDGE('',*,*,#2683,.F.);
#3423=ORIENTED_EDGE('',*,*,#2684,.T.);
#3424=ORIENTED_EDGE('',*,*,#2685,.T.);
#3425=ORIENTED_EDGE('',*,*,#2681,.F.);
#3426=ORIENTED_EDGE('',*,*,#2686,.F.);
#3427=ORIENTED_EDGE('',*,*,#2667,.T.);
#3428=ORIENTED_EDGE('',*,*,#2687,.T.);
#3429=ORIENTED_EDGE('',*,*,#2684,.F.);
#3430=ORIENTED_EDGE('',*,*,#2688,.F.);
#3431=ORIENTED_EDGE('',*,*,#2689,.T.);
#3432=ORIENTED_EDGE('',*,*,#2690,.T.);
#3433=ORIENTED_EDGE('',*,*,#2691,.F.);
#3434=ORIENTED_EDGE('',*,*,#2692,.F.);
#3435=ORIENTED_EDGE('',*,*,#2693,.T.);
#3436=ORIENTED_EDGE('',*,*,#2694,.T.);
#3437=ORIENTED_EDGE('',*,*,#2689,.F.);
#3438=ORIENTED_EDGE('',*,*,#2695,.F.);
#3439=ORIENTED_EDGE('',*,*,#2696,.T.);
#3440=ORIENTED_EDGE('',*,*,#2697,.T.);
#3441=ORIENTED_EDGE('',*,*,#2693,.F.);
#3442=ORIENTED_EDGE('',*,*,#2698,.F.);
#3443=ORIENTED_EDGE('',*,*,#2699,.T.);
#3444=ORIENTED_EDGE('',*,*,#2700,.T.);
#3445=ORIENTED_EDGE('',*,*,#2696,.F.);
#3446=ORIENTED_EDGE('',*,*,#2701,.F.);
#3447=ORIENTED_EDGE('',*,*,#2702,.T.);
#3448=ORIENTED_EDGE('',*,*,#2703,.T.);
#3449=ORIENTED_EDGE('',*,*,#2699,.F.);
#3450=ORIENTED_EDGE('',*,*,#2704,.F.);
#3451=ORIENTED_EDGE('',*,*,#2705,.T.);
#3452=ORIENTED_EDGE('',*,*,#2706,.T.);
#3453=ORIENTED_EDGE('',*,*,#2702,.F.);
#3454=ORIENTED_EDGE('',*,*,#2707,.F.);
#3455=ORIENTED_EDGE('',*,*,#2708,.T.);
#3456=ORIENTED_EDGE('',*,*,#2709,.T.);
#3457=ORIENTED_EDGE('',*,*,#2705,.F.);
#3458=ORIENTED_EDGE('',*,*,#2710,.F.);
#3459=ORIENTED_EDGE('',*,*,#2691,.T.);
#3460=ORIENTED_EDGE('',*,*,#2711,.T.);
#3461=ORIENTED_EDGE('',*,*,#2708,.F.);
#3462=ORIENTED_EDGE('',*,*,#2712,.F.);
#3463=ORIENTED_EDGE('',*,*,#2713,.T.);
#3464=ORIENTED_EDGE('',*,*,#2714,.T.);
#3465=ORIENTED_EDGE('',*,*,#2715,.F.);
#3466=ORIENTED_EDGE('',*,*,#2716,.F.);
#3467=ORIENTED_EDGE('',*,*,#2717,.T.);
#3468=ORIENTED_EDGE('',*,*,#2718,.T.);
#3469=ORIENTED_EDGE('',*,*,#2713,.F.);
#3470=ORIENTED_EDGE('',*,*,#2719,.F.);
#3471=ORIENTED_EDGE('',*,*,#2720,.T.);
#3472=ORIENTED_EDGE('',*,*,#2721,.T.);
#3473=ORIENTED_EDGE('',*,*,#2717,.F.);
#3474=ORIENTED_EDGE('',*,*,#2722,.F.);
#3475=ORIENTED_EDGE('',*,*,#2723,.T.);
#3476=ORIENTED_EDGE('',*,*,#2724,.T.);
#3477=ORIENTED_EDGE('',*,*,#2720,.F.);
#3478=ORIENTED_EDGE('',*,*,#2725,.F.);
#3479=ORIENTED_EDGE('',*,*,#2726,.T.);
#3480=ORIENTED_EDGE('',*,*,#2727,.T.);
#3481=ORIENTED_EDGE('',*,*,#2723,.F.);
#3482=ORIENTED_EDGE('',*,*,#2728,.F.);
#3483=ORIENTED_EDGE('',*,*,#2729,.T.);
#3484=ORIENTED_EDGE('',*,*,#2730,.T.);
#3485=ORIENTED_EDGE('',*,*,#2726,.F.);
#3486=ORIENTED_EDGE('',*,*,#2731,.F.);
#3487=ORIENTED_EDGE('',*,*,#2732,.T.);
#3488=ORIENTED_EDGE('',*,*,#2733,.T.);
#3489=ORIENTED_EDGE('',*,*,#2729,.F.);
#3490=ORIENTED_EDGE('',*,*,#2734,.F.);
#3491=ORIENTED_EDGE('',*,*,#2715,.T.);
#3492=ORIENTED_EDGE('',*,*,#2735,.T.);
#3493=ORIENTED_EDGE('',*,*,#2732,.F.);
#3494=ORIENTED_EDGE('',*,*,#2736,.F.);
#3495=ORIENTED_EDGE('',*,*,#2737,.T.);
#3496=ORIENTED_EDGE('',*,*,#2738,.T.);
#3497=ORIENTED_EDGE('',*,*,#2739,.F.);
#3498=ORIENTED_EDGE('',*,*,#2740,.F.);
#3499=ORIENTED_EDGE('',*,*,#2741,.T.);
#3500=ORIENTED_EDGE('',*,*,#2742,.T.);
#3501=ORIENTED_EDGE('',*,*,#2737,.F.);
#3502=ORIENTED_EDGE('',*,*,#2743,.F.);
#3503=ORIENTED_EDGE('',*,*,#2744,.T.);
#3504=ORIENTED_EDGE('',*,*,#2745,.T.);
#3505=ORIENTED_EDGE('',*,*,#2741,.F.);
#3506=ORIENTED_EDGE('',*,*,#2746,.F.);
#3507=ORIENTED_EDGE('',*,*,#2747,.T.);
#3508=ORIENTED_EDGE('',*,*,#2748,.T.);
#3509=ORIENTED_EDGE('',*,*,#2744,.F.);
#3510=ORIENTED_EDGE('',*,*,#2749,.F.);
#3511=ORIENTED_EDGE('',*,*,#2750,.T.);
#3512=ORIENTED_EDGE('',*,*,#2751,.T.);
#3513=ORIENTED_EDGE('',*,*,#2747,.F.);
#3514=ORIENTED_EDGE('',*,*,#2752,.F.);
#3515=ORIENTED_EDGE('',*,*,#2753,.T.);
#3516=ORIENTED_EDGE('',*,*,#2754,.T.);
#3517=ORIENTED_EDGE('',*,*,#2750,.F.);
#3518=ORIENTED_EDGE('',*,*,#2755,.F.);
#3519=ORIENTED_EDGE('',*,*,#2756,.T.);
#3520=ORIENTED_EDGE('',*,*,#2757,.T.);
#3521=ORIENTED_EDGE('',*,*,#2753,.F.);
#3522=ORIENTED_EDGE('',*,*,#2758,.F.);
#3523=ORIENTED_EDGE('',*,*,#2739,.T.);
#3524=ORIENTED_EDGE('',*,*,#2759,.T.);
#3525=ORIENTED_EDGE('',*,*,#2756,.F.);
#3526=ORIENTED_EDGE('',*,*,#2760,.F.);
#3527=ORIENTED_EDGE('',*,*,#2761,.T.);
#3528=ORIENTED_EDGE('',*,*,#2762,.T.);
#3529=ORIENTED_EDGE('',*,*,#2761,.F.);
#3530=ORIENTED_EDGE('',*,*,#2763,.T.);
#3531=ORIENTED_EDGE('',*,*,#2764,.T.);
#3532=ORIENTED_EDGE('',*,*,#2765,.T.);
#3533=ORIENTED_EDGE('',*,*,#2764,.F.);
#3534=ORIENTED_EDGE('',*,*,#2766,.T.);
#3535=ORIENTED_EDGE('',*,*,#2767,.T.);
#3536=ORIENTED_EDGE('',*,*,#2768,.T.);
#3537=ORIENTED_EDGE('',*,*,#2769,.T.);
#3538=ORIENTED_EDGE('',*,*,#2770,.T.);
#3539=ORIENTED_EDGE('',*,*,#2771,.T.);
#3540=ORIENTED_EDGE('',*,*,#2768,.F.);
#3541=ORIENTED_EDGE('',*,*,#2772,.T.);
#3542=ORIENTED_EDGE('',*,*,#2773,.T.);
#3543=ORIENTED_EDGE('',*,*,#2774,.T.);
#3544=ORIENTED_EDGE('',*,*,#2770,.F.);
#3545=ORIENTED_EDGE('',*,*,#2775,.T.);
#3546=ORIENTED_EDGE('',*,*,#2776,.T.);
#3547=ORIENTED_EDGE('',*,*,#2777,.T.);
#3548=ORIENTED_EDGE('',*,*,#2773,.F.);
#3549=ORIENTED_EDGE('',*,*,#2778,.T.);
#3550=ORIENTED_EDGE('',*,*,#2779,.T.);
#3551=ORIENTED_EDGE('',*,*,#2780,.T.);
#3552=ORIENTED_EDGE('',*,*,#2776,.F.);
#3553=ORIENTED_EDGE('',*,*,#2781,.T.);
#3554=ORIENTED_EDGE('',*,*,#2782,.T.);
#3555=ORIENTED_EDGE('',*,*,#2783,.T.);
#3556=ORIENTED_EDGE('',*,*,#2779,.F.);
#3557=ORIENTED_EDGE('',*,*,#2784,.T.);
#3558=ORIENTED_EDGE('',*,*,#2785,.T.);
#3559=ORIENTED_EDGE('',*,*,#2786,.T.);
#3560=ORIENTED_EDGE('',*,*,#2782,.F.);
#3561=ORIENTED_EDGE('',*,*,#2787,.T.);
#3562=ORIENTED_EDGE('',*,*,#2788,.T.);
#3563=ORIENTED_EDGE('',*,*,#2789,.T.);
#3564=ORIENTED_EDGE('',*,*,#2785,.F.);
#3565=ORIENTED_EDGE('',*,*,#2790,.T.);
#3566=ORIENTED_EDGE('',*,*,#2791,.T.);
#3567=ORIENTED_EDGE('',*,*,#2792,.T.);
#3568=ORIENTED_EDGE('',*,*,#2788,.F.);
#3569=ORIENTED_EDGE('',*,*,#2793,.T.);
#3570=ORIENTED_EDGE('',*,*,#2794,.T.);
#3571=ORIENTED_EDGE('',*,*,#2795,.T.);
#3572=ORIENTED_EDGE('',*,*,#2791,.F.);
#3573=ORIENTED_EDGE('',*,*,#2796,.T.);
#3574=ORIENTED_EDGE('',*,*,#2797,.T.);
#3575=ORIENTED_EDGE('',*,*,#2798,.T.);
#3576=ORIENTED_EDGE('',*,*,#2794,.F.);
#3577=ORIENTED_EDGE('',*,*,#2799,.T.);
#3578=ORIENTED_EDGE('',*,*,#2800,.T.);
#3579=ORIENTED_EDGE('',*,*,#2801,.T.);
#3580=ORIENTED_EDGE('',*,*,#2797,.F.);
#3581=ORIENTED_EDGE('',*,*,#2802,.T.);
#3582=ORIENTED_EDGE('',*,*,#2803,.T.);
#3583=ORIENTED_EDGE('',*,*,#2804,.T.);
#3584=ORIENTED_EDGE('',*,*,#2800,.F.);
#3585=ORIENTED_EDGE('',*,*,#2805,.T.);
#3586=ORIENTED_EDGE('',*,*,#2806,.T.);
#3587=ORIENTED_EDGE('',*,*,#2807,.T.);
#3588=ORIENTED_EDGE('',*,*,#2803,.F.);
#3589=ORIENTED_EDGE('',*,*,#2808,.T.);
#3590=ORIENTED_EDGE('',*,*,#2809,.T.);
#3591=ORIENTED_EDGE('',*,*,#2810,.T.);
#3592=ORIENTED_EDGE('',*,*,#2806,.F.);
#3593=ORIENTED_EDGE('',*,*,#2811,.T.);
#3594=ORIENTED_EDGE('',*,*,#2812,.T.);
#3595=ORIENTED_EDGE('',*,*,#2813,.T.);
#3596=ORIENTED_EDGE('',*,*,#2809,.F.);
#3597=ORIENTED_EDGE('',*,*,#2814,.T.);
#3598=ORIENTED_EDGE('',*,*,#2815,.T.);
#3599=ORIENTED_EDGE('',*,*,#2816,.T.);
#3600=ORIENTED_EDGE('',*,*,#2812,.F.);
#3601=ORIENTED_EDGE('',*,*,#2817,.T.);
#3602=ORIENTED_EDGE('',*,*,#2815,.F.);
#3603=ORIENTED_EDGE('',*,*,#2818,.T.);
#3604=ORIENTED_EDGE('',*,*,#2819,.T.);
#3605=ORIENTED_EDGE('',*,*,#2820,.T.);
#3606=ORIENTED_EDGE('',*,*,#2819,.F.);
#3607=ORIENTED_EDGE('',*,*,#2821,.T.);
#3608=ORIENTED_EDGE('',*,*,#2822,.T.);
#3609=ORIENTED_EDGE('',*,*,#2823,.T.);
#3610=ORIENTED_EDGE('',*,*,#2822,.F.);
#3611=ORIENTED_EDGE('',*,*,#2824,.T.);
#3612=ORIENTED_EDGE('',*,*,#2825,.T.);
#3613=ORIENTED_EDGE('',*,*,#2826,.T.);
#3614=ORIENTED_EDGE('',*,*,#2825,.F.);
#3615=ORIENTED_EDGE('',*,*,#2827,.T.);
#3616=ORIENTED_EDGE('',*,*,#2828,.T.);
#3617=ORIENTED_EDGE('',*,*,#2829,.T.);
#3618=ORIENTED_EDGE('',*,*,#2828,.F.);
#3619=ORIENTED_EDGE('',*,*,#2830,.T.);
#3620=ORIENTED_EDGE('',*,*,#2831,.T.);
#3621=ORIENTED_EDGE('',*,*,#2832,.T.);
#3622=ORIENTED_EDGE('',*,*,#2831,.F.);
#3623=ORIENTED_EDGE('',*,*,#2833,.T.);
#3624=ORIENTED_EDGE('',*,*,#2834,.T.);
#3625=ORIENTED_EDGE('',*,*,#2835,.T.);
#3626=ORIENTED_EDGE('',*,*,#2834,.F.);
#3627=ORIENTED_EDGE('',*,*,#2836,.T.);
#3628=ORIENTED_EDGE('',*,*,#2837,.T.);
#3629=ORIENTED_EDGE('',*,*,#2838,.T.);
#3630=ORIENTED_EDGE('',*,*,#2837,.F.);
#3631=ORIENTED_EDGE('',*,*,#2839,.T.);
#3632=ORIENTED_EDGE('',*,*,#2840,.T.);
#3633=ORIENTED_EDGE('',*,*,#2841,.T.);
#3634=ORIENTED_EDGE('',*,*,#2840,.F.);
#3635=ORIENTED_EDGE('',*,*,#2842,.T.);
#3636=ORIENTED_EDGE('',*,*,#2843,.T.);
#3637=ORIENTED_EDGE('',*,*,#2844,.T.);
#3638=ORIENTED_EDGE('',*,*,#2843,.F.);
#3639=ORIENTED_EDGE('',*,*,#2845,.T.);
#3640=ORIENTED_EDGE('',*,*,#2846,.T.);
#3641=ORIENTED_EDGE('',*,*,#2847,.T.);
#3642=ORIENTED_EDGE('',*,*,#2846,.F.);
#3643=ORIENTED_EDGE('',*,*,#2848,.T.);
#3644=ORIENTED_EDGE('',*,*,#2849,.T.);
#3645=ORIENTED_EDGE('',*,*,#2850,.T.);
#3646=ORIENTED_EDGE('',*,*,#2849,.F.);
#3647=ORIENTED_EDGE('',*,*,#2851,.T.);
#3648=ORIENTED_EDGE('',*,*,#2852,.T.);
#3649=ORIENTED_EDGE('',*,*,#2853,.T.);
#3650=ORIENTED_EDGE('',*,*,#2852,.F.);
#3651=ORIENTED_EDGE('',*,*,#2854,.T.);
#3652=ORIENTED_EDGE('',*,*,#2855,.T.);
#3653=ORIENTED_EDGE('',*,*,#2856,.T.);
#3654=ORIENTED_EDGE('',*,*,#2855,.F.);
#3655=ORIENTED_EDGE('',*,*,#2857,.T.);
#3656=ORIENTED_EDGE('',*,*,#2858,.T.);
#3657=ORIENTED_EDGE('',*,*,#2859,.T.);
#3658=ORIENTED_EDGE('',*,*,#2858,.F.);
#3659=ORIENTED_EDGE('',*,*,#2860,.T.);
#3660=ORIENTED_EDGE('',*,*,#2861,.T.);
#3661=ORIENTED_EDGE('',*,*,#2862,.T.);
#3662=ORIENTED_EDGE('',*,*,#2861,.F.);
#3663=ORIENTED_EDGE('',*,*,#2863,.T.);
#3664=ORIENTED_EDGE('',*,*,#2864,.T.);
#3665=ORIENTED_EDGE('',*,*,#2865,.T.);
#3666=ORIENTED_EDGE('',*,*,#2866,.T.);
#3667=ORIENTED_EDGE('',*,*,#2867,.T.);
#3668=ORIENTED_EDGE('',*,*,#2864,.F.);
#3669=ORIENTED_EDGE('',*,*,#2868,.T.);
#3670=ORIENTED_EDGE('',*,*,#2766,.F.);
#3671=ORIENTED_EDGE('',*,*,#2869,.T.);
#3672=ORIENTED_EDGE('',*,*,#2866,.F.);
#3673=ORIENTED_EDGE('',*,*,#2870,.T.);
#3674=ORIENTED_EDGE('',*,*,#2823,.F.);
#3675=ORIENTED_EDGE('',*,*,#2871,.F.);
#3676=ORIENTED_EDGE('',*,*,#2872,.F.);
#3677=ORIENTED_EDGE('',*,*,#2873,.T.);
#3678=ORIENTED_EDGE('',*,*,#2826,.F.);
#3679=ORIENTED_EDGE('',*,*,#2874,.F.);
#3680=ORIENTED_EDGE('',*,*,#2875,.F.);
#3681=ORIENTED_EDGE('',*,*,#2871,.T.);
#3682=ORIENTED_EDGE('',*,*,#2829,.F.);
#3683=ORIENTED_EDGE('',*,*,#2876,.F.);
#3684=ORIENTED_EDGE('',*,*,#2877,.F.);
#3685=ORIENTED_EDGE('',*,*,#2874,.T.);
#3686=ORIENTED_EDGE('',*,*,#2832,.F.);
#3687=ORIENTED_EDGE('',*,*,#2878,.F.);
#3688=ORIENTED_EDGE('',*,*,#2879,.F.);
#3689=ORIENTED_EDGE('',*,*,#2876,.T.);
#3690=ORIENTED_EDGE('',*,*,#2835,.F.);
#3691=ORIENTED_EDGE('',*,*,#2880,.F.);
#3692=ORIENTED_EDGE('',*,*,#2881,.F.);
#3693=ORIENTED_EDGE('',*,*,#2878,.T.);
#3694=ORIENTED_EDGE('',*,*,#2838,.F.);
#3695=ORIENTED_EDGE('',*,*,#2882,.F.);
#3696=ORIENTED_EDGE('',*,*,#2883,.F.);
#3697=ORIENTED_EDGE('',*,*,#2880,.T.);
#3698=ORIENTED_EDGE('',*,*,#2841,.F.);
#3699=ORIENTED_EDGE('',*,*,#2884,.F.);
#3700=ORIENTED_EDGE('',*,*,#2885,.F.);
#3701=ORIENTED_EDGE('',*,*,#2882,.T.);
#3702=ORIENTED_EDGE('',*,*,#2844,.F.);
#3703=ORIENTED_EDGE('',*,*,#2886,.F.);
#3704=ORIENTED_EDGE('',*,*,#2887,.F.);
#3705=ORIENTED_EDGE('',*,*,#2884,.T.);
#3706=ORIENTED_EDGE('',*,*,#2847,.F.);
#3707=ORIENTED_EDGE('',*,*,#2888,.F.);
#3708=ORIENTED_EDGE('',*,*,#2889,.F.);
#3709=ORIENTED_EDGE('',*,*,#2886,.T.);
#3710=ORIENTED_EDGE('',*,*,#2850,.F.);
#3711=ORIENTED_EDGE('',*,*,#2890,.F.);
#3712=ORIENTED_EDGE('',*,*,#2891,.F.);
#3713=ORIENTED_EDGE('',*,*,#2888,.T.);
#3714=ORIENTED_EDGE('',*,*,#2853,.F.);
#3715=ORIENTED_EDGE('',*,*,#2892,.F.);
#3716=ORIENTED_EDGE('',*,*,#2893,.F.);
#3717=ORIENTED_EDGE('',*,*,#2890,.T.);
#3718=ORIENTED_EDGE('',*,*,#2856,.F.);
#3719=ORIENTED_EDGE('',*,*,#2894,.F.);
#3720=ORIENTED_EDGE('',*,*,#2895,.F.);
#3721=ORIENTED_EDGE('',*,*,#2892,.T.);
#3722=ORIENTED_EDGE('',*,*,#2859,.F.);
#3723=ORIENTED_EDGE('',*,*,#2896,.F.);
#3724=ORIENTED_EDGE('',*,*,#2897,.F.);
#3725=ORIENTED_EDGE('',*,*,#2894,.T.);
#3726=ORIENTED_EDGE('',*,*,#2862,.F.);
#3727=ORIENTED_EDGE('',*,*,#2898,.F.);
#3728=ORIENTED_EDGE('',*,*,#2899,.F.);
#3729=ORIENTED_EDGE('',*,*,#2896,.T.);
#3730=ORIENTED_EDGE('',*,*,#2865,.F.);
#3731=ORIENTED_EDGE('',*,*,#2900,.F.);
#3732=ORIENTED_EDGE('',*,*,#2901,.F.);
#3733=ORIENTED_EDGE('',*,*,#2898,.T.);
#3734=ORIENTED_EDGE('',*,*,#2867,.F.);
#3735=ORIENTED_EDGE('',*,*,#2902,.T.);
#3736=ORIENTED_EDGE('',*,*,#2903,.F.);
#3737=ORIENTED_EDGE('',*,*,#2900,.T.);
#3738=ORIENTED_EDGE('',*,*,#2869,.F.);
#3739=ORIENTED_EDGE('',*,*,#2904,.F.);
#3740=ORIENTED_EDGE('',*,*,#2905,.F.);
#3741=ORIENTED_EDGE('',*,*,#2902,.F.);
#3742=ORIENTED_EDGE('',*,*,#2769,.F.);
#3743=ORIENTED_EDGE('',*,*,#2906,.F.);
#3744=ORIENTED_EDGE('',*,*,#2907,.F.);
#3745=ORIENTED_EDGE('',*,*,#2904,.T.);
#3746=ORIENTED_EDGE('',*,*,#2767,.F.);
#3747=ORIENTED_EDGE('',*,*,#2870,.F.);
#3748=ORIENTED_EDGE('',*,*,#2868,.F.);
#3749=ORIENTED_EDGE('',*,*,#2863,.F.);
#3750=ORIENTED_EDGE('',*,*,#2860,.F.);
#3751=ORIENTED_EDGE('',*,*,#2857,.F.);
#3752=ORIENTED_EDGE('',*,*,#2854,.F.);
#3753=ORIENTED_EDGE('',*,*,#2851,.F.);
#3754=ORIENTED_EDGE('',*,*,#2848,.F.);
#3755=ORIENTED_EDGE('',*,*,#2845,.F.);
#3756=ORIENTED_EDGE('',*,*,#2842,.F.);
#3757=ORIENTED_EDGE('',*,*,#2839,.F.);
#3758=ORIENTED_EDGE('',*,*,#2836,.F.);
#3759=ORIENTED_EDGE('',*,*,#2833,.F.);
#3760=ORIENTED_EDGE('',*,*,#2830,.F.);
#3761=ORIENTED_EDGE('',*,*,#2827,.F.);
#3762=ORIENTED_EDGE('',*,*,#2824,.F.);
#3763=ORIENTED_EDGE('',*,*,#2821,.F.);
#3764=ORIENTED_EDGE('',*,*,#2818,.F.);
#3765=ORIENTED_EDGE('',*,*,#2817,.F.);
#3766=ORIENTED_EDGE('',*,*,#2814,.F.);
#3767=ORIENTED_EDGE('',*,*,#2811,.F.);
#3768=ORIENTED_EDGE('',*,*,#2808,.F.);
#3769=ORIENTED_EDGE('',*,*,#2805,.F.);
#3770=ORIENTED_EDGE('',*,*,#2802,.F.);
#3771=ORIENTED_EDGE('',*,*,#2799,.F.);
#3772=ORIENTED_EDGE('',*,*,#2796,.F.);
#3773=ORIENTED_EDGE('',*,*,#2793,.F.);
#3774=ORIENTED_EDGE('',*,*,#2790,.F.);
#3775=ORIENTED_EDGE('',*,*,#2787,.F.);
#3776=ORIENTED_EDGE('',*,*,#2784,.F.);
#3777=ORIENTED_EDGE('',*,*,#2781,.F.);
#3778=ORIENTED_EDGE('',*,*,#2778,.F.);
#3779=ORIENTED_EDGE('',*,*,#2775,.F.);
#3780=ORIENTED_EDGE('',*,*,#2772,.F.);
#3781=ORIENTED_EDGE('',*,*,#2908,.F.);
#3782=ORIENTED_EDGE('',*,*,#2909,.F.);
#3783=ORIENTED_EDGE('',*,*,#2910,.F.);
#3784=ORIENTED_EDGE('',*,*,#2763,.F.);
#3785=ORIENTED_EDGE('',*,*,#2911,.T.);
#3786=ORIENTED_EDGE('',*,*,#2760,.T.);
#3787=ORIENTED_EDGE('',*,*,#2912,.F.);
#3788=ORIENTED_EDGE('',*,*,#2913,.T.);
#3789=ORIENTED_EDGE('',*,*,#2914,.T.);
#3790=ORIENTED_EDGE('',*,*,#2915,.T.);
#3791=ORIENTED_EDGE('',*,*,#2905,.T.);
#3792=ORIENTED_EDGE('',*,*,#2916,.T.);
#3793=ORIENTED_EDGE('',*,*,#2903,.T.);
#3794=ORIENTED_EDGE('',*,*,#2915,.F.);
#3795=ORIENTED_EDGE('',*,*,#2917,.T.);
#3796=ORIENTED_EDGE('',*,*,#2918,.T.);
#3797=ORIENTED_EDGE('',*,*,#2901,.T.);
#3798=ORIENTED_EDGE('',*,*,#2916,.F.);
#3799=ORIENTED_EDGE('',*,*,#2919,.T.);
#3800=ORIENTED_EDGE('',*,*,#2920,.T.);
#3801=ORIENTED_EDGE('',*,*,#2899,.T.);
#3802=ORIENTED_EDGE('',*,*,#2918,.F.);
#3803=ORIENTED_EDGE('',*,*,#2921,.T.);
#3804=ORIENTED_EDGE('',*,*,#2920,.F.);
#3805=ORIENTED_EDGE('',*,*,#2922,.T.);
#3806=ORIENTED_EDGE('',*,*,#2923,.T.);
#3807=ORIENTED_EDGE('',*,*,#2897,.T.);
#3808=ORIENTED_EDGE('',*,*,#2924,.T.);
#3809=ORIENTED_EDGE('',*,*,#2895,.T.);
#3810=ORIENTED_EDGE('',*,*,#2923,.F.);
#3811=ORIENTED_EDGE('',*,*,#2925,.T.);
#3812=ORIENTED_EDGE('',*,*,#2924,.F.);
#3813=ORIENTED_EDGE('',*,*,#2926,.T.);
#3814=ORIENTED_EDGE('',*,*,#2927,.T.);
#3815=ORIENTED_EDGE('',*,*,#2893,.T.);
#3816=ORIENTED_EDGE('',*,*,#2928,.T.);
#3817=ORIENTED_EDGE('',*,*,#2891,.T.);
#3818=ORIENTED_EDGE('',*,*,#2927,.F.);
#3819=ORIENTED_EDGE('',*,*,#2929,.T.);
#3820=ORIENTED_EDGE('',*,*,#2928,.F.);
#3821=ORIENTED_EDGE('',*,*,#2930,.T.);
#3822=ORIENTED_EDGE('',*,*,#2931,.T.);
#3823=ORIENTED_EDGE('',*,*,#2889,.T.);
#3824=ORIENTED_EDGE('',*,*,#2932,.T.);
#3825=ORIENTED_EDGE('',*,*,#2887,.T.);
#3826=ORIENTED_EDGE('',*,*,#2931,.F.);
#3827=ORIENTED_EDGE('',*,*,#2933,.T.);
#3828=ORIENTED_EDGE('',*,*,#2932,.F.);
#3829=ORIENTED_EDGE('',*,*,#2934,.T.);
#3830=ORIENTED_EDGE('',*,*,#2935,.T.);
#3831=ORIENTED_EDGE('',*,*,#2885,.T.);
#3832=ORIENTED_EDGE('',*,*,#2936,.T.);
#3833=ORIENTED_EDGE('',*,*,#2883,.T.);
#3834=ORIENTED_EDGE('',*,*,#2935,.F.);
#3835=ORIENTED_EDGE('',*,*,#2937,.T.);
#3836=ORIENTED_EDGE('',*,*,#2936,.F.);
#3837=ORIENTED_EDGE('',*,*,#2938,.T.);
#3838=ORIENTED_EDGE('',*,*,#2939,.T.);
#3839=ORIENTED_EDGE('',*,*,#2881,.T.);
#3840=ORIENTED_EDGE('',*,*,#2940,.T.);
#3841=ORIENTED_EDGE('',*,*,#2879,.T.);
#3842=ORIENTED_EDGE('',*,*,#2939,.F.);
#3843=ORIENTED_EDGE('',*,*,#2941,.T.);
#3844=ORIENTED_EDGE('',*,*,#2942,.T.);
#3845=ORIENTED_EDGE('',*,*,#2877,.T.);
#3846=ORIENTED_EDGE('',*,*,#2940,.F.);
#3847=ORIENTED_EDGE('',*,*,#2943,.T.);
#3848=ORIENTED_EDGE('',*,*,#2944,.T.);
#3849=ORIENTED_EDGE('',*,*,#2875,.T.);
#3850=ORIENTED_EDGE('',*,*,#2942,.F.);
#3851=ORIENTED_EDGE('',*,*,#2945,.T.);
#3852=ORIENTED_EDGE('',*,*,#2946,.T.);
#3853=ORIENTED_EDGE('',*,*,#2872,.T.);
#3854=ORIENTED_EDGE('',*,*,#2944,.F.);
#3855=ORIENTED_EDGE('',*,*,#2947,.T.);
#3856=ORIENTED_EDGE('',*,*,#2948,.T.);
#3857=ORIENTED_EDGE('',*,*,#2949,.T.);
#3858=ORIENTED_EDGE('',*,*,#2946,.F.);
#3859=ORIENTED_EDGE('',*,*,#2950,.T.);
#3860=ORIENTED_EDGE('',*,*,#2948,.F.);
#3861=ORIENTED_EDGE('',*,*,#2951,.T.);
#3862=ORIENTED_EDGE('',*,*,#2952,.T.);
#3863=ORIENTED_EDGE('',*,*,#2953,.T.);
#3864=ORIENTED_EDGE('',*,*,#2952,.F.);
#3865=ORIENTED_EDGE('',*,*,#2954,.T.);
#3866=ORIENTED_EDGE('',*,*,#2955,.T.);
#3867=ORIENTED_EDGE('',*,*,#2956,.T.);
#3868=ORIENTED_EDGE('',*,*,#2955,.F.);
#3869=ORIENTED_EDGE('',*,*,#2957,.T.);
#3870=ORIENTED_EDGE('',*,*,#2958,.T.);
#3871=ORIENTED_EDGE('',*,*,#2959,.T.);
#3872=ORIENTED_EDGE('',*,*,#2958,.F.);
#3873=ORIENTED_EDGE('',*,*,#2960,.T.);
#3874=ORIENTED_EDGE('',*,*,#2961,.T.);
#3875=ORIENTED_EDGE('',*,*,#2962,.T.);
#3876=ORIENTED_EDGE('',*,*,#2963,.T.);
#3877=ORIENTED_EDGE('',*,*,#2964,.T.);
#3878=ORIENTED_EDGE('',*,*,#2961,.F.);
#3879=ORIENTED_EDGE('',*,*,#2965,.T.);
#3880=ORIENTED_EDGE('',*,*,#2963,.F.);
#3881=ORIENTED_EDGE('',*,*,#2966,.T.);
#3882=ORIENTED_EDGE('',*,*,#2967,.T.);
#3883=ORIENTED_EDGE('',*,*,#2968,.T.);
#3884=ORIENTED_EDGE('',*,*,#2969,.T.);
#3885=ORIENTED_EDGE('',*,*,#2970,.T.);
#3886=ORIENTED_EDGE('',*,*,#2967,.F.);
#3887=ORIENTED_EDGE('',*,*,#2971,.T.);
#3888=ORIENTED_EDGE('',*,*,#2969,.F.);
#3889=ORIENTED_EDGE('',*,*,#2972,.T.);
#3890=ORIENTED_EDGE('',*,*,#2973,.T.);
#3891=ORIENTED_EDGE('',*,*,#2974,.T.);
#3892=ORIENTED_EDGE('',*,*,#2975,.T.);
#3893=ORIENTED_EDGE('',*,*,#2976,.T.);
#3894=ORIENTED_EDGE('',*,*,#2973,.F.);
#3895=ORIENTED_EDGE('',*,*,#2977,.T.);
#3896=ORIENTED_EDGE('',*,*,#2975,.F.);
#3897=ORIENTED_EDGE('',*,*,#2978,.T.);
#3898=ORIENTED_EDGE('',*,*,#2979,.T.);
#3899=ORIENTED_EDGE('',*,*,#2980,.T.);
#3900=ORIENTED_EDGE('',*,*,#2981,.T.);
#3901=ORIENTED_EDGE('',*,*,#2982,.T.);
#3902=ORIENTED_EDGE('',*,*,#2979,.F.);
#3903=ORIENTED_EDGE('',*,*,#2983,.T.);
#3904=ORIENTED_EDGE('',*,*,#2981,.F.);
#3905=ORIENTED_EDGE('',*,*,#2984,.T.);
#3906=ORIENTED_EDGE('',*,*,#2985,.T.);
#3907=ORIENTED_EDGE('',*,*,#2986,.T.);
#3908=ORIENTED_EDGE('',*,*,#2987,.T.);
#3909=ORIENTED_EDGE('',*,*,#2988,.T.);
#3910=ORIENTED_EDGE('',*,*,#2985,.F.);
#3911=ORIENTED_EDGE('',*,*,#2989,.T.);
#3912=ORIENTED_EDGE('',*,*,#2987,.F.);
#3913=ORIENTED_EDGE('',*,*,#2990,.T.);
#3914=ORIENTED_EDGE('',*,*,#2991,.T.);
#3915=ORIENTED_EDGE('',*,*,#2992,.T.);
#3916=ORIENTED_EDGE('',*,*,#2991,.F.);
#3917=ORIENTED_EDGE('',*,*,#2993,.T.);
#3918=ORIENTED_EDGE('',*,*,#2994,.T.);
#3919=ORIENTED_EDGE('',*,*,#2995,.T.);
#3920=ORIENTED_EDGE('',*,*,#2996,.T.);
#3921=ORIENTED_EDGE('',*,*,#2997,.T.);
#3922=ORIENTED_EDGE('',*,*,#2994,.F.);
#3923=ORIENTED_EDGE('',*,*,#2998,.T.);
#3924=ORIENTED_EDGE('',*,*,#2913,.F.);
#3925=ORIENTED_EDGE('',*,*,#2907,.T.);
#3926=ORIENTED_EDGE('',*,*,#2996,.F.);
#3927=ORIENTED_EDGE('',*,*,#2999,.T.);
#3928=ORIENTED_EDGE('',*,*,#2816,.F.);
#3929=ORIENTED_EDGE('',*,*,#3000,.F.);
#3930=ORIENTED_EDGE('',*,*,#2953,.F.);
#3931=ORIENTED_EDGE('',*,*,#3001,.T.);
#3932=ORIENTED_EDGE('',*,*,#2813,.F.);
#3933=ORIENTED_EDGE('',*,*,#3001,.F.);
#3934=ORIENTED_EDGE('',*,*,#2956,.F.);
#3935=ORIENTED_EDGE('',*,*,#3002,.T.);
#3936=ORIENTED_EDGE('',*,*,#2810,.F.);
#3937=ORIENTED_EDGE('',*,*,#3002,.F.);
#3938=ORIENTED_EDGE('',*,*,#2959,.F.);
#3939=ORIENTED_EDGE('',*,*,#3003,.T.);
#3940=ORIENTED_EDGE('',*,*,#2807,.F.);
#3941=ORIENTED_EDGE('',*,*,#3003,.F.);
#3942=ORIENTED_EDGE('',*,*,#2962,.F.);
#3943=ORIENTED_EDGE('',*,*,#3004,.T.);
#3944=ORIENTED_EDGE('',*,*,#2804,.F.);
#3945=ORIENTED_EDGE('',*,*,#3004,.F.);
#3946=ORIENTED_EDGE('',*,*,#2964,.F.);
#3947=ORIENTED_EDGE('',*,*,#3005,.T.);
#3948=ORIENTED_EDGE('',*,*,#2801,.F.);
#3949=ORIENTED_EDGE('',*,*,#3005,.F.);
#3950=ORIENTED_EDGE('',*,*,#2968,.F.);
#3951=ORIENTED_EDGE('',*,*,#3006,.T.);
#3952=ORIENTED_EDGE('',*,*,#2798,.F.);
#3953=ORIENTED_EDGE('',*,*,#3006,.F.);
#3954=ORIENTED_EDGE('',*,*,#2970,.F.);
#3955=ORIENTED_EDGE('',*,*,#3007,.T.);
#3956=ORIENTED_EDGE('',*,*,#2795,.F.);
#3957=ORIENTED_EDGE('',*,*,#3007,.F.);
#3958=ORIENTED_EDGE('',*,*,#2974,.F.);
#3959=ORIENTED_EDGE('',*,*,#3008,.T.);
#3960=ORIENTED_EDGE('',*,*,#2792,.F.);
#3961=ORIENTED_EDGE('',*,*,#3008,.F.);
#3962=ORIENTED_EDGE('',*,*,#2976,.F.);
#3963=ORIENTED_EDGE('',*,*,#3009,.T.);
#3964=ORIENTED_EDGE('',*,*,#2789,.F.);
#3965=ORIENTED_EDGE('',*,*,#3009,.F.);
#3966=ORIENTED_EDGE('',*,*,#2980,.F.);
#3967=ORIENTED_EDGE('',*,*,#3010,.T.);
#3968=ORIENTED_EDGE('',*,*,#2786,.F.);
#3969=ORIENTED_EDGE('',*,*,#3010,.F.);
#3970=ORIENTED_EDGE('',*,*,#2982,.F.);
#3971=ORIENTED_EDGE('',*,*,#3011,.T.);
#3972=ORIENTED_EDGE('',*,*,#2783,.F.);
#3973=ORIENTED_EDGE('',*,*,#3011,.F.);
#3974=ORIENTED_EDGE('',*,*,#2986,.F.);
#3975=ORIENTED_EDGE('',*,*,#3012,.T.);
#3976=ORIENTED_EDGE('',*,*,#2780,.F.);
#3977=ORIENTED_EDGE('',*,*,#3012,.F.);
#3978=ORIENTED_EDGE('',*,*,#2988,.F.);
#3979=ORIENTED_EDGE('',*,*,#3013,.T.);
#3980=ORIENTED_EDGE('',*,*,#2777,.F.);
#3981=ORIENTED_EDGE('',*,*,#3013,.F.);
#3982=ORIENTED_EDGE('',*,*,#2992,.F.);
#3983=ORIENTED_EDGE('',*,*,#3014,.T.);
#3984=ORIENTED_EDGE('',*,*,#2774,.F.);
#3985=ORIENTED_EDGE('',*,*,#3014,.F.);
#3986=ORIENTED_EDGE('',*,*,#2995,.F.);
#3987=ORIENTED_EDGE('',*,*,#3015,.F.);
#3988=ORIENTED_EDGE('',*,*,#2771,.F.);
#3989=ORIENTED_EDGE('',*,*,#3015,.T.);
#3990=ORIENTED_EDGE('',*,*,#2997,.F.);
#3991=ORIENTED_EDGE('',*,*,#2906,.T.);
#3992=ORIENTED_EDGE('',*,*,#2914,.F.);
#3993=ORIENTED_EDGE('',*,*,#2999,.F.);
#3994=ORIENTED_EDGE('',*,*,#2998,.F.);
#3995=ORIENTED_EDGE('',*,*,#2993,.F.);
#3996=ORIENTED_EDGE('',*,*,#2990,.F.);
#3997=ORIENTED_EDGE('',*,*,#2989,.F.);
#3998=ORIENTED_EDGE('',*,*,#2984,.F.);
#3999=ORIENTED_EDGE('',*,*,#2983,.F.);
#4000=ORIENTED_EDGE('',*,*,#2978,.F.);
#4001=ORIENTED_EDGE('',*,*,#2977,.F.);
#4002=ORIENTED_EDGE('',*,*,#2972,.F.);
#4003=ORIENTED_EDGE('',*,*,#2971,.F.);
#4004=ORIENTED_EDGE('',*,*,#2966,.F.);
#4005=ORIENTED_EDGE('',*,*,#2965,.F.);
#4006=ORIENTED_EDGE('',*,*,#2960,.F.);
#4007=ORIENTED_EDGE('',*,*,#2957,.F.);
#4008=ORIENTED_EDGE('',*,*,#2954,.F.);
#4009=ORIENTED_EDGE('',*,*,#2951,.F.);
#4010=ORIENTED_EDGE('',*,*,#2950,.F.);
#4011=ORIENTED_EDGE('',*,*,#2947,.F.);
#4012=ORIENTED_EDGE('',*,*,#2945,.F.);
#4013=ORIENTED_EDGE('',*,*,#2943,.F.);
#4014=ORIENTED_EDGE('',*,*,#2941,.F.);
#4015=ORIENTED_EDGE('',*,*,#2938,.F.);
#4016=ORIENTED_EDGE('',*,*,#2937,.F.);
#4017=ORIENTED_EDGE('',*,*,#2934,.F.);
#4018=ORIENTED_EDGE('',*,*,#2933,.F.);
#4019=ORIENTED_EDGE('',*,*,#2930,.F.);
#4020=ORIENTED_EDGE('',*,*,#2929,.F.);
#4021=ORIENTED_EDGE('',*,*,#2926,.F.);
#4022=ORIENTED_EDGE('',*,*,#2925,.F.);
#4023=ORIENTED_EDGE('',*,*,#2922,.F.);
#4024=ORIENTED_EDGE('',*,*,#2921,.F.);
#4025=ORIENTED_EDGE('',*,*,#2919,.F.);
#4026=ORIENTED_EDGE('',*,*,#2917,.F.);
#4027=ORIENTED_EDGE('',*,*,#3016,.F.);
#4028=ORIENTED_EDGE('',*,*,#3017,.T.);
#4029=ORIENTED_EDGE('',*,*,#3018,.F.);
#4030=ORIENTED_EDGE('',*,*,#2736,.T.);
#4031=ORIENTED_EDGE('',*,*,#2758,.T.);
#4032=ORIENTED_EDGE('',*,*,#2755,.T.);
#4033=ORIENTED_EDGE('',*,*,#2752,.T.);
#4034=ORIENTED_EDGE('',*,*,#2749,.T.);
#4035=ORIENTED_EDGE('',*,*,#2746,.T.);
#4036=ORIENTED_EDGE('',*,*,#2743,.T.);
#4037=ORIENTED_EDGE('',*,*,#2740,.T.);
#4038=ORIENTED_EDGE('',*,*,#2712,.T.);
#4039=ORIENTED_EDGE('',*,*,#2734,.T.);
#4040=ORIENTED_EDGE('',*,*,#2731,.T.);
#4041=ORIENTED_EDGE('',*,*,#2728,.T.);
#4042=ORIENTED_EDGE('',*,*,#2725,.T.);
#4043=ORIENTED_EDGE('',*,*,#2722,.T.);
#4044=ORIENTED_EDGE('',*,*,#2719,.T.);
#4045=ORIENTED_EDGE('',*,*,#2716,.T.);
#4046=ORIENTED_EDGE('',*,*,#2688,.T.);
#4047=ORIENTED_EDGE('',*,*,#2710,.T.);
#4048=ORIENTED_EDGE('',*,*,#2707,.T.);
#4049=ORIENTED_EDGE('',*,*,#2704,.T.);
#4050=ORIENTED_EDGE('',*,*,#2701,.T.);
#4051=ORIENTED_EDGE('',*,*,#2698,.T.);
#4052=ORIENTED_EDGE('',*,*,#2695,.T.);
#4053=ORIENTED_EDGE('',*,*,#2692,.T.);
#4054=ORIENTED_EDGE('',*,*,#2664,.T.);
#4055=ORIENTED_EDGE('',*,*,#2686,.T.);
#4056=ORIENTED_EDGE('',*,*,#2683,.T.);
#4057=ORIENTED_EDGE('',*,*,#2680,.T.);
#4058=ORIENTED_EDGE('',*,*,#2677,.T.);
#4059=ORIENTED_EDGE('',*,*,#2674,.T.);
#4060=ORIENTED_EDGE('',*,*,#2671,.T.);
#4061=ORIENTED_EDGE('',*,*,#2668,.T.);
#4062=ORIENTED_EDGE('',*,*,#2711,.F.);
#4063=ORIENTED_EDGE('',*,*,#2690,.F.);
#4064=ORIENTED_EDGE('',*,*,#2694,.F.);
#4065=ORIENTED_EDGE('',*,*,#2697,.F.);
#4066=ORIENTED_EDGE('',*,*,#2700,.F.);
#4067=ORIENTED_EDGE('',*,*,#2703,.F.);
#4068=ORIENTED_EDGE('',*,*,#2706,.F.);
#4069=ORIENTED_EDGE('',*,*,#2709,.F.);
#4070=ORIENTED_EDGE('',*,*,#3019,.F.);
#4071=ORIENTED_EDGE('',*,*,#2687,.F.);
#4072=ORIENTED_EDGE('',*,*,#2666,.F.);
#4073=ORIENTED_EDGE('',*,*,#2670,.F.);
#4074=ORIENTED_EDGE('',*,*,#2673,.F.);
#4075=ORIENTED_EDGE('',*,*,#2676,.F.);
#4076=ORIENTED_EDGE('',*,*,#2679,.F.);
#4077=ORIENTED_EDGE('',*,*,#2682,.F.);
#4078=ORIENTED_EDGE('',*,*,#2685,.F.);
#4079=ORIENTED_EDGE('',*,*,#2762,.F.);
#4080=ORIENTED_EDGE('',*,*,#2759,.F.);
#4081=ORIENTED_EDGE('',*,*,#2738,.F.);
#4082=ORIENTED_EDGE('',*,*,#2742,.F.);
#4083=ORIENTED_EDGE('',*,*,#2745,.F.);
#4084=ORIENTED_EDGE('',*,*,#2748,.F.);
#4085=ORIENTED_EDGE('',*,*,#2751,.F.);
#4086=ORIENTED_EDGE('',*,*,#2754,.F.);
#4087=ORIENTED_EDGE('',*,*,#2757,.F.);
#4088=ORIENTED_EDGE('',*,*,#2765,.F.);
#4089=ORIENTED_EDGE('',*,*,#2735,.F.);
#4090=ORIENTED_EDGE('',*,*,#2714,.F.);
#4091=ORIENTED_EDGE('',*,*,#2718,.F.);
#4092=ORIENTED_EDGE('',*,*,#2721,.F.);
#4093=ORIENTED_EDGE('',*,*,#2724,.F.);
#4094=ORIENTED_EDGE('',*,*,#2727,.F.);
#4095=ORIENTED_EDGE('',*,*,#2730,.F.);
#4096=ORIENTED_EDGE('',*,*,#2733,.F.);
#4097=ORIENTED_EDGE('',*,*,#3020,.F.);
#4098=ORIENTED_EDGE('',*,*,#3021,.T.);
#4099=ORIENTED_EDGE('',*,*,#3022,.T.);
#4100=ORIENTED_EDGE('',*,*,#2908,.T.);
#4101=ORIENTED_EDGE('',*,*,#3022,.F.);
#4102=ORIENTED_EDGE('',*,*,#3021,.F.);
#4103=ORIENTED_EDGE('',*,*,#3023,.T.);
#4104=ORIENTED_EDGE('',*,*,#3017,.F.);
#4105=ORIENTED_EDGE('',*,*,#3023,.F.);
#4106=ORIENTED_EDGE('',*,*,#3024,.T.);
#4107=ORIENTED_EDGE('',*,*,#3025,.T.);
#4108=ORIENTED_EDGE('',*,*,#2912,.T.);
#4109=ORIENTED_EDGE('',*,*,#3025,.F.);
#4110=ORIENTED_EDGE('',*,*,#3024,.F.);
#4111=ORIENTED_EDGE('',*,*,#3026,.T.);
#4112=ORIENTED_EDGE('',*,*,#3018,.T.);
#4113=ORIENTED_EDGE('',*,*,#3026,.F.);
#4114=ORIENTED_EDGE('',*,*,#2909,.T.);
#4115=ORIENTED_EDGE('',*,*,#3027,.T.);
#4116=ORIENTED_EDGE('',*,*,#3028,.T.);
#4117=ORIENTED_EDGE('',*,*,#3027,.F.);
#4118=ORIENTED_EDGE('',*,*,#3028,.F.);
#4119=ORIENTED_EDGE('',*,*,#3029,.T.);
#4120=ORIENTED_EDGE('',*,*,#3016,.T.);
#4121=ORIENTED_EDGE('',*,*,#3029,.F.);
#4122=ORIENTED_EDGE('',*,*,#2910,.T.);
#4123=ORIENTED_EDGE('',*,*,#3030,.T.);
#4124=ORIENTED_EDGE('',*,*,#3019,.T.);
#4125=ORIENTED_EDGE('',*,*,#3030,.F.);
#4126=ORIENTED_EDGE('',*,*,#2911,.F.);
#4127=ORIENTED_EDGE('',*,*,#3031,.T.);
#4128=ORIENTED_EDGE('',*,*,#3020,.T.);
#4129=ORIENTED_EDGE('',*,*,#3031,.F.);
#4130=ORIENTED_EDGE('',*,*,#2820,.F.);
#4131=ORIENTED_EDGE('',*,*,#2873,.F.);
#4132=ORIENTED_EDGE('',*,*,#2949,.F.);
#4133=ORIENTED_EDGE('',*,*,#3000,.T.);
#4134=ORIENTED_EDGE('',*,*,#3032,.T.);
#4135=ORIENTED_EDGE('',*,*,#3033,.T.);
#4136=ORIENTED_EDGE('',*,*,#3034,.T.);
#4137=ORIENTED_EDGE('',*,*,#3033,.F.);
#4138=ORIENTED_EDGE('',*,*,#3034,.F.);
#4139=ORIENTED_EDGE('',*,*,#3035,.T.);
#4140=ORIENTED_EDGE('',*,*,#3036,.F.);
#4141=ORIENTED_EDGE('',*,*,#3035,.F.);
#4142=ORIENTED_EDGE('',*,*,#3032,.F.);
#4143=ORIENTED_EDGE('',*,*,#3036,.T.);
#4144=ORIENTED_EDGE('',*,*,#3037,.T.);
#4145=ORIENTED_EDGE('',*,*,#3038,.T.);
#4146=ORIENTED_EDGE('',*,*,#3037,.F.);
#4147=ORIENTED_EDGE('',*,*,#3038,.F.);
#4148=ORIENTED_EDGE('',*,*,#3039,.F.);
#4149=ORIENTED_EDGE('',*,*,#3040,.T.);
#4150=ORIENTED_EDGE('',*,*,#3039,.T.);
#4151=ORIENTED_EDGE('',*,*,#3040,.F.);
#4152=ORIENTED_EDGE('',*,*,#3041,.T.);
#4153=ORIENTED_EDGE('',*,*,#3042,.F.);
#4154=ORIENTED_EDGE('',*,*,#3042,.T.);
#4155=ORIENTED_EDGE('',*,*,#3043,.T.);
#4156=ORIENTED_EDGE('',*,*,#3044,.F.);
#4157=ORIENTED_EDGE('',*,*,#3043,.F.);
#4158=ORIENTED_EDGE('',*,*,#3041,.F.);
#4159=ORIENTED_EDGE('',*,*,#3044,.T.);
#4160=ORIENTED_EDGE('',*,*,#3045,.F.);
#4161=ORIENTED_EDGE('',*,*,#3046,.F.);
#4162=ORIENTED_EDGE('',*,*,#3046,.T.);
#4163=ORIENTED_EDGE('',*,*,#3047,.T.);
#4164=ORIENTED_EDGE('',*,*,#3048,.T.);
#4165=ORIENTED_EDGE('',*,*,#3049,.T.);
#4166=ORIENTED_EDGE('',*,*,#3048,.F.);
#4167=ORIENTED_EDGE('',*,*,#3049,.F.);
#4168=ORIENTED_EDGE('',*,*,#3050,.T.);
#4169=ORIENTED_EDGE('',*,*,#3051,.F.);
#4170=ORIENTED_EDGE('',*,*,#3050,.F.);
#4171=ORIENTED_EDGE('',*,*,#3047,.F.);
#4172=ORIENTED_EDGE('',*,*,#3045,.T.);
#4173=ORIENTED_EDGE('',*,*,#3052,.F.);
#4174=ORIENTED_EDGE('',*,*,#3053,.T.);
#4175=ORIENTED_EDGE('',*,*,#3054,.T.);
#4176=ORIENTED_EDGE('',*,*,#3055,.F.);
#4177=ORIENTED_EDGE('',*,*,#3056,.F.);
#4178=ORIENTED_EDGE('',*,*,#3057,.T.);
#4179=ORIENTED_EDGE('',*,*,#3058,.T.);
#4180=ORIENTED_EDGE('',*,*,#3053,.F.);
#4181=ORIENTED_EDGE('',*,*,#3059,.F.);
#4182=ORIENTED_EDGE('',*,*,#3060,.T.);
#4183=ORIENTED_EDGE('',*,*,#3061,.T.);
#4184=ORIENTED_EDGE('',*,*,#3057,.F.);
#4185=ORIENTED_EDGE('',*,*,#3062,.F.);
#4186=ORIENTED_EDGE('',*,*,#3063,.T.);
#4187=ORIENTED_EDGE('',*,*,#3064,.T.);
#4188=ORIENTED_EDGE('',*,*,#3060,.F.);
#4189=ORIENTED_EDGE('',*,*,#3065,.F.);
#4190=ORIENTED_EDGE('',*,*,#3066,.T.);
#4191=ORIENTED_EDGE('',*,*,#3067,.T.);
#4192=ORIENTED_EDGE('',*,*,#3063,.F.);
#4193=ORIENTED_EDGE('',*,*,#3068,.F.);
#4194=ORIENTED_EDGE('',*,*,#3055,.T.);
#4195=ORIENTED_EDGE('',*,*,#3069,.T.);
#4196=ORIENTED_EDGE('',*,*,#3066,.F.);
#4197=ORIENTED_EDGE('',*,*,#3069,.F.);
#4198=ORIENTED_EDGE('',*,*,#3054,.F.);
#4199=ORIENTED_EDGE('',*,*,#3058,.F.);
#4200=ORIENTED_EDGE('',*,*,#3061,.F.);
#4201=ORIENTED_EDGE('',*,*,#3064,.F.);
#4202=ORIENTED_EDGE('',*,*,#3067,.F.);
#4203=ORIENTED_EDGE('',*,*,#3070,.T.);
#4204=ORIENTED_EDGE('',*,*,#3071,.T.);
#4205=ORIENTED_EDGE('',*,*,#3051,.T.);
#4206=ORIENTED_EDGE('',*,*,#3071,.F.);
#4207=ORIENTED_EDGE('',*,*,#3070,.F.);
#4208=ORIENTED_EDGE('',*,*,#3052,.T.);
#4209=ORIENTED_EDGE('',*,*,#3068,.T.);
#4210=ORIENTED_EDGE('',*,*,#3065,.T.);
#4211=ORIENTED_EDGE('',*,*,#3062,.T.);
#4212=ORIENTED_EDGE('',*,*,#3059,.T.);
#4213=ORIENTED_EDGE('',*,*,#3056,.T.);
#4214=ORIENTED_EDGE('',*,*,#3072,.F.);
#4215=ORIENTED_EDGE('',*,*,#3073,.T.);
#4216=ORIENTED_EDGE('',*,*,#3073,.F.);
#4217=ORIENTED_EDGE('',*,*,#3074,.F.);
#4218=ORIENTED_EDGE('',*,*,#3075,.F.);
#4219=ORIENTED_EDGE('',*,*,#3076,.F.);
#4220=ORIENTED_EDGE('',*,*,#3077,.F.);
#4221=ORIENTED_EDGE('',*,*,#3078,.F.);
#4222=ORIENTED_EDGE('',*,*,#3079,.F.);
#4223=ORIENTED_EDGE('',*,*,#3080,.F.);
#4224=ORIENTED_EDGE('',*,*,#3081,.F.);
#4225=ORIENTED_EDGE('',*,*,#3082,.F.);
#4226=ORIENTED_EDGE('',*,*,#3083,.F.);
#4227=ORIENTED_EDGE('',*,*,#3084,.F.);
#4228=ORIENTED_EDGE('',*,*,#3085,.F.);
#4229=ORIENTED_EDGE('',*,*,#3086,.F.);
#4230=ORIENTED_EDGE('',*,*,#3087,.F.);
#4231=ORIENTED_EDGE('',*,*,#3088,.F.);
#4232=ORIENTED_EDGE('',*,*,#3089,.F.);
#4233=ORIENTED_EDGE('',*,*,#3090,.F.);
#4234=ORIENTED_EDGE('',*,*,#3091,.F.);
#4235=ORIENTED_EDGE('',*,*,#3092,.F.);
#4236=ORIENTED_EDGE('',*,*,#3093,.F.);
#4237=ORIENTED_EDGE('',*,*,#3094,.F.);
#4238=ORIENTED_EDGE('',*,*,#3095,.F.);
#4239=ORIENTED_EDGE('',*,*,#3096,.F.);
#4240=ORIENTED_EDGE('',*,*,#3097,.F.);
#4241=ORIENTED_EDGE('',*,*,#3098,.F.);
#4242=ORIENTED_EDGE('',*,*,#3099,.F.);
#4243=ORIENTED_EDGE('',*,*,#3100,.F.);
#4244=ORIENTED_EDGE('',*,*,#3101,.F.);
#4245=ORIENTED_EDGE('',*,*,#3102,.F.);
#4246=ORIENTED_EDGE('',*,*,#3103,.F.);
#4247=ORIENTED_EDGE('',*,*,#3104,.T.);
#4248=ORIENTED_EDGE('',*,*,#3105,.F.);
#4249=ORIENTED_EDGE('',*,*,#3106,.F.);
#4250=ORIENTED_EDGE('',*,*,#3107,.T.);
#4251=ORIENTED_EDGE('',*,*,#3108,.T.);
#4252=ORIENTED_EDGE('',*,*,#3072,.T.);
#4253=ORIENTED_EDGE('',*,*,#3108,.F.);
#4254=ORIENTED_EDGE('',*,*,#3109,.T.);
#4255=ORIENTED_EDGE('',*,*,#3109,.F.);
#4256=ORIENTED_EDGE('',*,*,#3107,.F.);
#4257=ORIENTED_EDGE('',*,*,#3110,.T.);
#4258=ORIENTED_EDGE('',*,*,#3110,.F.);
#4259=ORIENTED_EDGE('',*,*,#3106,.T.);
#4260=ORIENTED_EDGE('',*,*,#3111,.T.);
#4261=ORIENTED_EDGE('',*,*,#3112,.T.);
#4262=ORIENTED_EDGE('',*,*,#3111,.F.);
#4263=ORIENTED_EDGE('',*,*,#3113,.F.);
#4264=ORIENTED_EDGE('',*,*,#3114,.T.);
#4265=ORIENTED_EDGE('',*,*,#3112,.F.);
#4266=ORIENTED_EDGE('',*,*,#3114,.F.);
#4267=ORIENTED_EDGE('',*,*,#3102,.T.);
#4268=ORIENTED_EDGE('',*,*,#3115,.T.);
#4269=ORIENTED_EDGE('',*,*,#3116,.T.);
#4270=ORIENTED_EDGE('',*,*,#3115,.F.);
#4271=ORIENTED_EDGE('',*,*,#3117,.F.);
#4272=ORIENTED_EDGE('',*,*,#3118,.T.);
#4273=ORIENTED_EDGE('',*,*,#3116,.F.);
#4274=ORIENTED_EDGE('',*,*,#3118,.F.);
#4275=ORIENTED_EDGE('',*,*,#3119,.T.);
#4276=ORIENTED_EDGE('',*,*,#3120,.T.);
#4277=ORIENTED_EDGE('',*,*,#3105,.T.);
#4278=ORIENTED_EDGE('',*,*,#3120,.F.);
#4279=ORIENTED_EDGE('',*,*,#3121,.F.);
#4280=ORIENTED_EDGE('',*,*,#3122,.T.);
#4281=ORIENTED_EDGE('',*,*,#3119,.F.);
#4282=ORIENTED_EDGE('',*,*,#3122,.F.);
#4283=ORIENTED_EDGE('',*,*,#3123,.T.);
#4284=ORIENTED_EDGE('',*,*,#3124,.T.);
#4285=ORIENTED_EDGE('',*,*,#3103,.T.);
#4286=ORIENTED_EDGE('',*,*,#3124,.F.);
#4287=ORIENTED_EDGE('',*,*,#3125,.F.);
#4288=ORIENTED_EDGE('',*,*,#3126,.T.);
#4289=ORIENTED_EDGE('',*,*,#3123,.F.);
#4290=ORIENTED_EDGE('',*,*,#3126,.F.);
#4291=ORIENTED_EDGE('',*,*,#3113,.T.);
#4292=ORIENTED_EDGE('',*,*,#3127,.T.);
#4293=ORIENTED_EDGE('',*,*,#3128,.T.);
#4294=ORIENTED_EDGE('',*,*,#3127,.F.);
#4295=ORIENTED_EDGE('',*,*,#3129,.F.);
#4296=ORIENTED_EDGE('',*,*,#3130,.F.);
#4297=ORIENTED_EDGE('',*,*,#3131,.F.);
#4298=ORIENTED_EDGE('',*,*,#3132,.F.);
#4299=ORIENTED_EDGE('',*,*,#3133,.F.);
#4300=ORIENTED_EDGE('',*,*,#3134,.F.);
#4301=ORIENTED_EDGE('',*,*,#3135,.F.);
#4302=ORIENTED_EDGE('',*,*,#3136,.F.);
#4303=ORIENTED_EDGE('',*,*,#3137,.F.);
#4304=ORIENTED_EDGE('',*,*,#3138,.F.);
#4305=ORIENTED_EDGE('',*,*,#3139,.F.);
#4306=ORIENTED_EDGE('',*,*,#3140,.F.);
#4307=ORIENTED_EDGE('',*,*,#3141,.F.);
#4308=ORIENTED_EDGE('',*,*,#3142,.F.);
#4309=ORIENTED_EDGE('',*,*,#3143,.F.);
#4310=ORIENTED_EDGE('',*,*,#3144,.F.);
#4311=ORIENTED_EDGE('',*,*,#3145,.F.);
#4312=ORIENTED_EDGE('',*,*,#3146,.F.);
#4313=ORIENTED_EDGE('',*,*,#3147,.F.);
#4314=ORIENTED_EDGE('',*,*,#3148,.F.);
#4315=ORIENTED_EDGE('',*,*,#3149,.F.);
#4316=ORIENTED_EDGE('',*,*,#3150,.F.);
#4317=ORIENTED_EDGE('',*,*,#3151,.F.);
#4318=ORIENTED_EDGE('',*,*,#3152,.F.);
#4319=ORIENTED_EDGE('',*,*,#3153,.F.);
#4320=ORIENTED_EDGE('',*,*,#3154,.F.);
#4321=ORIENTED_EDGE('',*,*,#3155,.F.);
#4322=ORIENTED_EDGE('',*,*,#3156,.F.);
#4323=ORIENTED_EDGE('',*,*,#3157,.F.);
#4324=ORIENTED_EDGE('',*,*,#3158,.F.);
#4325=ORIENTED_EDGE('',*,*,#3159,.T.);
#4326=ORIENTED_EDGE('',*,*,#3160,.F.);
#4327=ORIENTED_EDGE('',*,*,#3128,.F.);
#4328=ORIENTED_EDGE('',*,*,#3117,.T.);
#4329=ORIENTED_EDGE('',*,*,#3161,.T.);
#4330=ORIENTED_EDGE('',*,*,#3157,.T.);
#4331=ORIENTED_EDGE('',*,*,#3161,.F.);
#4332=ORIENTED_EDGE('',*,*,#3160,.T.);
#4333=ORIENTED_EDGE('',*,*,#3162,.T.);
#4334=ORIENTED_EDGE('',*,*,#3121,.T.);
#4335=ORIENTED_EDGE('',*,*,#3162,.F.);
#4336=ORIENTED_EDGE('',*,*,#3158,.T.);
#4337=ORIENTED_EDGE('',*,*,#3163,.T.);
#4338=ORIENTED_EDGE('',*,*,#3125,.T.);
#4339=ORIENTED_EDGE('',*,*,#3163,.F.);
#4340=ORIENTED_EDGE('',*,*,#3164,.T.);
#4341=ORIENTED_EDGE('',*,*,#3129,.T.);
#4342=ORIENTED_EDGE('',*,*,#3165,.T.);
#4343=ORIENTED_EDGE('',*,*,#3166,.T.);
#4344=ORIENTED_EDGE('',*,*,#3164,.F.);
#4345=ORIENTED_EDGE('',*,*,#3167,.T.);
#4346=ORIENTED_EDGE('',*,*,#3168,.T.);
#4347=ORIENTED_EDGE('',*,*,#3130,.T.);
#4348=ORIENTED_EDGE('',*,*,#3169,.T.);
#4349=ORIENTED_EDGE('',*,*,#3131,.T.);
#4350=ORIENTED_EDGE('',*,*,#3168,.F.);
#4351=ORIENTED_EDGE('',*,*,#3170,.T.);
#4352=ORIENTED_EDGE('',*,*,#3169,.F.);
#4353=ORIENTED_EDGE('',*,*,#3171,.T.);
#4354=ORIENTED_EDGE('',*,*,#3172,.T.);
#4355=ORIENTED_EDGE('',*,*,#3132,.T.);
#4356=ORIENTED_EDGE('',*,*,#3173,.T.);
#4357=ORIENTED_EDGE('',*,*,#3133,.T.);
#4358=ORIENTED_EDGE('',*,*,#3172,.F.);
#4359=ORIENTED_EDGE('',*,*,#3174,.T.);
#4360=ORIENTED_EDGE('',*,*,#3173,.F.);
#4361=ORIENTED_EDGE('',*,*,#3175,.T.);
#4362=ORIENTED_EDGE('',*,*,#3176,.T.);
#4363=ORIENTED_EDGE('',*,*,#3134,.T.);
#4364=ORIENTED_EDGE('',*,*,#3177,.T.);
#4365=ORIENTED_EDGE('',*,*,#3135,.T.);
#4366=ORIENTED_EDGE('',*,*,#3176,.F.);
#4367=ORIENTED_EDGE('',*,*,#3178,.T.);
#4368=ORIENTED_EDGE('',*,*,#3179,.T.);
#4369=ORIENTED_EDGE('',*,*,#3136,.T.);
#4370=ORIENTED_EDGE('',*,*,#3177,.F.);
#4371=ORIENTED_EDGE('',*,*,#3180,.T.);
#4372=ORIENTED_EDGE('',*,*,#3179,.F.);
#4373=ORIENTED_EDGE('',*,*,#3181,.T.);
#4374=ORIENTED_EDGE('',*,*,#3182,.T.);
#4375=ORIENTED_EDGE('',*,*,#3137,.T.);
#4376=ORIENTED_EDGE('',*,*,#3183,.T.);
#4377=ORIENTED_EDGE('',*,*,#3138,.T.);
#4378=ORIENTED_EDGE('',*,*,#3182,.F.);
#4379=ORIENTED_EDGE('',*,*,#3184,.T.);
#4380=ORIENTED_EDGE('',*,*,#3183,.F.);
#4381=ORIENTED_EDGE('',*,*,#3185,.T.);
#4382=ORIENTED_EDGE('',*,*,#3186,.T.);
#4383=ORIENTED_EDGE('',*,*,#3139,.T.);
#4384=ORIENTED_EDGE('',*,*,#3187,.T.);
#4385=ORIENTED_EDGE('',*,*,#3140,.T.);
#4386=ORIENTED_EDGE('',*,*,#3186,.F.);
#4387=ORIENTED_EDGE('',*,*,#3188,.T.);
#4388=ORIENTED_EDGE('',*,*,#3187,.F.);
#4389=ORIENTED_EDGE('',*,*,#3189,.T.);
#4390=ORIENTED_EDGE('',*,*,#3190,.T.);
#4391=ORIENTED_EDGE('',*,*,#3141,.T.);
#4392=ORIENTED_EDGE('',*,*,#3190,.F.);
#4393=ORIENTED_EDGE('',*,*,#3191,.T.);
#4394=ORIENTED_EDGE('',*,*,#3192,.T.);
#4395=ORIENTED_EDGE('',*,*,#3142,.T.);
#4396=ORIENTED_EDGE('',*,*,#3192,.F.);
#4397=ORIENTED_EDGE('',*,*,#3193,.T.);
#4398=ORIENTED_EDGE('',*,*,#3194,.T.);
#4399=ORIENTED_EDGE('',*,*,#3143,.T.);
#4400=ORIENTED_EDGE('',*,*,#3194,.F.);
#4401=ORIENTED_EDGE('',*,*,#3195,.T.);
#4402=ORIENTED_EDGE('',*,*,#3196,.T.);
#4403=ORIENTED_EDGE('',*,*,#3144,.T.);
#4404=ORIENTED_EDGE('',*,*,#3196,.F.);
#4405=ORIENTED_EDGE('',*,*,#3197,.T.);
#4406=ORIENTED_EDGE('',*,*,#3198,.T.);
#4407=ORIENTED_EDGE('',*,*,#3145,.T.);
#4408=ORIENTED_EDGE('',*,*,#3198,.F.);
#4409=ORIENTED_EDGE('',*,*,#3199,.T.);
#4410=ORIENTED_EDGE('',*,*,#3200,.T.);
#4411=ORIENTED_EDGE('',*,*,#3146,.T.);
#4412=ORIENTED_EDGE('',*,*,#3200,.F.);
#4413=ORIENTED_EDGE('',*,*,#3201,.T.);
#4414=ORIENTED_EDGE('',*,*,#3202,.T.);
#4415=ORIENTED_EDGE('',*,*,#3147,.T.);
#4416=ORIENTED_EDGE('',*,*,#3202,.F.);
#4417=ORIENTED_EDGE('',*,*,#3203,.T.);
#4418=ORIENTED_EDGE('',*,*,#3204,.T.);
#4419=ORIENTED_EDGE('',*,*,#3148,.T.);
#4420=ORIENTED_EDGE('',*,*,#3204,.F.);
#4421=ORIENTED_EDGE('',*,*,#3205,.T.);
#4422=ORIENTED_EDGE('',*,*,#3206,.T.);
#4423=ORIENTED_EDGE('',*,*,#3149,.T.);
#4424=ORIENTED_EDGE('',*,*,#3206,.F.);
#4425=ORIENTED_EDGE('',*,*,#3207,.T.);
#4426=ORIENTED_EDGE('',*,*,#3208,.T.);
#4427=ORIENTED_EDGE('',*,*,#3150,.T.);
#4428=ORIENTED_EDGE('',*,*,#3208,.F.);
#4429=ORIENTED_EDGE('',*,*,#3209,.T.);
#4430=ORIENTED_EDGE('',*,*,#3210,.T.);
#4431=ORIENTED_EDGE('',*,*,#3151,.T.);
#4432=ORIENTED_EDGE('',*,*,#3210,.F.);
#4433=ORIENTED_EDGE('',*,*,#3211,.T.);
#4434=ORIENTED_EDGE('',*,*,#3212,.T.);
#4435=ORIENTED_EDGE('',*,*,#3152,.T.);
#4436=ORIENTED_EDGE('',*,*,#3212,.F.);
#4437=ORIENTED_EDGE('',*,*,#3213,.T.);
#4438=ORIENTED_EDGE('',*,*,#3214,.T.);
#4439=ORIENTED_EDGE('',*,*,#3153,.T.);
#4440=ORIENTED_EDGE('',*,*,#3214,.F.);
#4441=ORIENTED_EDGE('',*,*,#3215,.T.);
#4442=ORIENTED_EDGE('',*,*,#3216,.T.);
#4443=ORIENTED_EDGE('',*,*,#3154,.T.);
#4444=ORIENTED_EDGE('',*,*,#3217,.T.);
#4445=ORIENTED_EDGE('',*,*,#3155,.T.);
#4446=ORIENTED_EDGE('',*,*,#3216,.F.);
#4447=ORIENTED_EDGE('',*,*,#3218,.T.);
#4448=ORIENTED_EDGE('',*,*,#3217,.F.);
#4449=ORIENTED_EDGE('',*,*,#3219,.T.);
#4450=ORIENTED_EDGE('',*,*,#3165,.F.);
#4451=ORIENTED_EDGE('',*,*,#3156,.T.);
#4452=ORIENTED_EDGE('',*,*,#3191,.F.);
#4453=ORIENTED_EDGE('',*,*,#3220,.F.);
#4454=ORIENTED_EDGE('',*,*,#3221,.F.);
#4455=ORIENTED_EDGE('',*,*,#3222,.F.);
#4456=ORIENTED_EDGE('',*,*,#3189,.F.);
#4457=ORIENTED_EDGE('',*,*,#3223,.T.);
#4458=ORIENTED_EDGE('',*,*,#3224,.F.);
#4459=ORIENTED_EDGE('',*,*,#3220,.T.);
#4460=ORIENTED_EDGE('',*,*,#3188,.F.);
#4461=ORIENTED_EDGE('',*,*,#3225,.F.);
#4462=ORIENTED_EDGE('',*,*,#3226,.F.);
#4463=ORIENTED_EDGE('',*,*,#3223,.F.);
#4464=ORIENTED_EDGE('',*,*,#3185,.F.);
#4465=ORIENTED_EDGE('',*,*,#3227,.T.);
#4466=ORIENTED_EDGE('',*,*,#3228,.F.);
#4467=ORIENTED_EDGE('',*,*,#3225,.T.);
#4468=ORIENTED_EDGE('',*,*,#3184,.F.);
#4469=ORIENTED_EDGE('',*,*,#3229,.F.);
#4470=ORIENTED_EDGE('',*,*,#3230,.F.);
#4471=ORIENTED_EDGE('',*,*,#3227,.F.);
#4472=ORIENTED_EDGE('',*,*,#3181,.F.);
#4473=ORIENTED_EDGE('',*,*,#3231,.T.);
#4474=ORIENTED_EDGE('',*,*,#3232,.F.);
#4475=ORIENTED_EDGE('',*,*,#3229,.T.);
#4476=ORIENTED_EDGE('',*,*,#3180,.F.);
#4477=ORIENTED_EDGE('',*,*,#3233,.F.);
#4478=ORIENTED_EDGE('',*,*,#3234,.F.);
#4479=ORIENTED_EDGE('',*,*,#3231,.F.);
#4480=ORIENTED_EDGE('',*,*,#3178,.F.);
#4481=ORIENTED_EDGE('',*,*,#3235,.F.);
#4482=ORIENTED_EDGE('',*,*,#3236,.F.);
#4483=ORIENTED_EDGE('',*,*,#3233,.T.);
#4484=ORIENTED_EDGE('',*,*,#3175,.F.);
#4485=ORIENTED_EDGE('',*,*,#3237,.T.);
#4486=ORIENTED_EDGE('',*,*,#3238,.F.);
#4487=ORIENTED_EDGE('',*,*,#3235,.T.);
#4488=ORIENTED_EDGE('',*,*,#3174,.F.);
#4489=ORIENTED_EDGE('',*,*,#3239,.F.);
#4490=ORIENTED_EDGE('',*,*,#3240,.F.);
#4491=ORIENTED_EDGE('',*,*,#3237,.F.);
#4492=ORIENTED_EDGE('',*,*,#3171,.F.);
#4493=ORIENTED_EDGE('',*,*,#3241,.T.);
#4494=ORIENTED_EDGE('',*,*,#3242,.F.);
#4495=ORIENTED_EDGE('',*,*,#3239,.T.);
#4496=ORIENTED_EDGE('',*,*,#3170,.F.);
#4497=ORIENTED_EDGE('',*,*,#3243,.F.);
#4498=ORIENTED_EDGE('',*,*,#3244,.F.);
#4499=ORIENTED_EDGE('',*,*,#3241,.F.);
#4500=ORIENTED_EDGE('',*,*,#3167,.F.);
#4501=ORIENTED_EDGE('',*,*,#3245,.T.);
#4502=ORIENTED_EDGE('',*,*,#3246,.F.);
#4503=ORIENTED_EDGE('',*,*,#3243,.T.);
#4504=ORIENTED_EDGE('',*,*,#3166,.F.);
#4505=ORIENTED_EDGE('',*,*,#3247,.F.);
#4506=ORIENTED_EDGE('',*,*,#3248,.F.);
#4507=ORIENTED_EDGE('',*,*,#3245,.F.);
#4508=ORIENTED_EDGE('',*,*,#3249,.T.);
#4509=ORIENTED_EDGE('',*,*,#3248,.T.);
#4510=ORIENTED_EDGE('',*,*,#3250,.T.);
#4511=ORIENTED_EDGE('',*,*,#3074,.T.);
#4512=ORIENTED_EDGE('',*,*,#3251,.T.);
#4513=ORIENTED_EDGE('',*,*,#3246,.T.);
#4514=ORIENTED_EDGE('',*,*,#3249,.F.);
#4515=ORIENTED_EDGE('',*,*,#3101,.T.);
#4516=ORIENTED_EDGE('',*,*,#3252,.T.);
#4517=ORIENTED_EDGE('',*,*,#3244,.T.);
#4518=ORIENTED_EDGE('',*,*,#3251,.F.);
#4519=ORIENTED_EDGE('',*,*,#3100,.T.);
#4520=ORIENTED_EDGE('',*,*,#3253,.T.);
#4521=ORIENTED_EDGE('',*,*,#3242,.T.);
#4522=ORIENTED_EDGE('',*,*,#3252,.F.);
#4523=ORIENTED_EDGE('',*,*,#3099,.T.);
#4524=ORIENTED_EDGE('',*,*,#3254,.T.);
#4525=ORIENTED_EDGE('',*,*,#3240,.T.);
#4526=ORIENTED_EDGE('',*,*,#3253,.F.);
#4527=ORIENTED_EDGE('',*,*,#3098,.T.);
#4528=ORIENTED_EDGE('',*,*,#3255,.T.);
#4529=ORIENTED_EDGE('',*,*,#3238,.T.);
#4530=ORIENTED_EDGE('',*,*,#3254,.F.);
#4531=ORIENTED_EDGE('',*,*,#3097,.T.);
#4532=ORIENTED_EDGE('',*,*,#3256,.T.);
#4533=ORIENTED_EDGE('',*,*,#3236,.T.);
#4534=ORIENTED_EDGE('',*,*,#3255,.F.);
#4535=ORIENTED_EDGE('',*,*,#3096,.T.);
#4536=ORIENTED_EDGE('',*,*,#3257,.T.);
#4537=ORIENTED_EDGE('',*,*,#3234,.T.);
#4538=ORIENTED_EDGE('',*,*,#3256,.F.);
#4539=ORIENTED_EDGE('',*,*,#3095,.T.);
#4540=ORIENTED_EDGE('',*,*,#3258,.T.);
#4541=ORIENTED_EDGE('',*,*,#3232,.T.);
#4542=ORIENTED_EDGE('',*,*,#3257,.F.);
#4543=ORIENTED_EDGE('',*,*,#3094,.T.);
#4544=ORIENTED_EDGE('',*,*,#3259,.T.);
#4545=ORIENTED_EDGE('',*,*,#3230,.T.);
#4546=ORIENTED_EDGE('',*,*,#3258,.F.);
#4547=ORIENTED_EDGE('',*,*,#3093,.T.);
#4548=ORIENTED_EDGE('',*,*,#3260,.T.);
#4549=ORIENTED_EDGE('',*,*,#3228,.T.);
#4550=ORIENTED_EDGE('',*,*,#3259,.F.);
#4551=ORIENTED_EDGE('',*,*,#3092,.T.);
#4552=ORIENTED_EDGE('',*,*,#3260,.F.);
#4553=ORIENTED_EDGE('',*,*,#3091,.T.);
#4554=ORIENTED_EDGE('',*,*,#3261,.T.);
#4555=ORIENTED_EDGE('',*,*,#3226,.T.);
#4556=ORIENTED_EDGE('',*,*,#3262,.T.);
#4557=ORIENTED_EDGE('',*,*,#3224,.T.);
#4558=ORIENTED_EDGE('',*,*,#3261,.F.);
#4559=ORIENTED_EDGE('',*,*,#3090,.T.);
#4560=ORIENTED_EDGE('',*,*,#3262,.F.);
#4561=ORIENTED_EDGE('',*,*,#3089,.T.);
#4562=ORIENTED_EDGE('',*,*,#3263,.T.);
#4563=ORIENTED_EDGE('',*,*,#3221,.T.);
#4564=ORIENTED_EDGE('',*,*,#3264,.T.);
#4565=ORIENTED_EDGE('',*,*,#3265,.T.);
#4566=ORIENTED_EDGE('',*,*,#3263,.F.);
#4567=ORIENTED_EDGE('',*,*,#3088,.T.);
#4568=ORIENTED_EDGE('',*,*,#3264,.F.);
#4569=ORIENTED_EDGE('',*,*,#3087,.T.);
#4570=ORIENTED_EDGE('',*,*,#3266,.T.);
#4571=ORIENTED_EDGE('',*,*,#3267,.T.);
#4572=ORIENTED_EDGE('',*,*,#3266,.F.);
#4573=ORIENTED_EDGE('',*,*,#3086,.T.);
#4574=ORIENTED_EDGE('',*,*,#3268,.T.);
#4575=ORIENTED_EDGE('',*,*,#3269,.T.);
#4576=ORIENTED_EDGE('',*,*,#3270,.T.);
#4577=ORIENTED_EDGE('',*,*,#3271,.T.);
#4578=ORIENTED_EDGE('',*,*,#3268,.F.);
#4579=ORIENTED_EDGE('',*,*,#3085,.T.);
#4580=ORIENTED_EDGE('',*,*,#3270,.F.);
#4581=ORIENTED_EDGE('',*,*,#3084,.T.);
#4582=ORIENTED_EDGE('',*,*,#3272,.T.);
#4583=ORIENTED_EDGE('',*,*,#3273,.T.);
#4584=ORIENTED_EDGE('',*,*,#3274,.T.);
#4585=ORIENTED_EDGE('',*,*,#3275,.T.);
#4586=ORIENTED_EDGE('',*,*,#3272,.F.);
#4587=ORIENTED_EDGE('',*,*,#3083,.T.);
#4588=ORIENTED_EDGE('',*,*,#3274,.F.);
#4589=ORIENTED_EDGE('',*,*,#3082,.T.);
#4590=ORIENTED_EDGE('',*,*,#3276,.T.);
#4591=ORIENTED_EDGE('',*,*,#3277,.T.);
#4592=ORIENTED_EDGE('',*,*,#3278,.T.);
#4593=ORIENTED_EDGE('',*,*,#3279,.T.);
#4594=ORIENTED_EDGE('',*,*,#3276,.F.);
#4595=ORIENTED_EDGE('',*,*,#3081,.T.);
#4596=ORIENTED_EDGE('',*,*,#3278,.F.);
#4597=ORIENTED_EDGE('',*,*,#3080,.T.);
#4598=ORIENTED_EDGE('',*,*,#3280,.T.);
#4599=ORIENTED_EDGE('',*,*,#3281,.T.);
#4600=ORIENTED_EDGE('',*,*,#3282,.T.);
#4601=ORIENTED_EDGE('',*,*,#3283,.T.);
#4602=ORIENTED_EDGE('',*,*,#3280,.F.);
#4603=ORIENTED_EDGE('',*,*,#3079,.T.);
#4604=ORIENTED_EDGE('',*,*,#3282,.F.);
#4605=ORIENTED_EDGE('',*,*,#3078,.T.);
#4606=ORIENTED_EDGE('',*,*,#3284,.T.);
#4607=ORIENTED_EDGE('',*,*,#3285,.T.);
#4608=ORIENTED_EDGE('',*,*,#3286,.T.);
#4609=ORIENTED_EDGE('',*,*,#3287,.T.);
#4610=ORIENTED_EDGE('',*,*,#3284,.F.);
#4611=ORIENTED_EDGE('',*,*,#3077,.T.);
#4612=ORIENTED_EDGE('',*,*,#3288,.T.);
#4613=ORIENTED_EDGE('',*,*,#3289,.T.);
#4614=ORIENTED_EDGE('',*,*,#3286,.F.);
#4615=ORIENTED_EDGE('',*,*,#3076,.T.);
#4616=ORIENTED_EDGE('',*,*,#3250,.F.);
#4617=ORIENTED_EDGE('',*,*,#3290,.T.);
#4618=ORIENTED_EDGE('',*,*,#3288,.F.);
#4619=ORIENTED_EDGE('',*,*,#3075,.T.);
#4620=ORIENTED_EDGE('',*,*,#3195,.F.);
#4621=ORIENTED_EDGE('',*,*,#3291,.F.);
#4622=ORIENTED_EDGE('',*,*,#3267,.F.);
#4623=ORIENTED_EDGE('',*,*,#3292,.T.);
#4624=ORIENTED_EDGE('',*,*,#3197,.F.);
#4625=ORIENTED_EDGE('',*,*,#3292,.F.);
#4626=ORIENTED_EDGE('',*,*,#3269,.F.);
#4627=ORIENTED_EDGE('',*,*,#3293,.F.);
#4628=ORIENTED_EDGE('',*,*,#3199,.F.);
#4629=ORIENTED_EDGE('',*,*,#3293,.T.);
#4630=ORIENTED_EDGE('',*,*,#3271,.F.);
#4631=ORIENTED_EDGE('',*,*,#3294,.T.);
#4632=ORIENTED_EDGE('',*,*,#3201,.F.);
#4633=ORIENTED_EDGE('',*,*,#3294,.F.);
#4634=ORIENTED_EDGE('',*,*,#3273,.F.);
#4635=ORIENTED_EDGE('',*,*,#3295,.F.);
#4636=ORIENTED_EDGE('',*,*,#3203,.F.);
#4637=ORIENTED_EDGE('',*,*,#3295,.T.);
#4638=ORIENTED_EDGE('',*,*,#3275,.F.);
#4639=ORIENTED_EDGE('',*,*,#3296,.T.);
#4640=ORIENTED_EDGE('',*,*,#3205,.F.);
#4641=ORIENTED_EDGE('',*,*,#3296,.F.);
#4642=ORIENTED_EDGE('',*,*,#3277,.F.);
#4643=ORIENTED_EDGE('',*,*,#3297,.F.);
#4644=ORIENTED_EDGE('',*,*,#3207,.F.);
#4645=ORIENTED_EDGE('',*,*,#3297,.T.);
#4646=ORIENTED_EDGE('',*,*,#3279,.F.);
#4647=ORIENTED_EDGE('',*,*,#3298,.T.);
#4648=ORIENTED_EDGE('',*,*,#3209,.F.);
#4649=ORIENTED_EDGE('',*,*,#3298,.F.);
#4650=ORIENTED_EDGE('',*,*,#3281,.F.);
#4651=ORIENTED_EDGE('',*,*,#3299,.F.);
#4652=ORIENTED_EDGE('',*,*,#3211,.F.);
#4653=ORIENTED_EDGE('',*,*,#3299,.T.);
#4654=ORIENTED_EDGE('',*,*,#3283,.F.);
#4655=ORIENTED_EDGE('',*,*,#3300,.T.);
#4656=ORIENTED_EDGE('',*,*,#3213,.F.);
#4657=ORIENTED_EDGE('',*,*,#3300,.F.);
#4658=ORIENTED_EDGE('',*,*,#3285,.F.);
#4659=ORIENTED_EDGE('',*,*,#3301,.T.);
#4660=ORIENTED_EDGE('',*,*,#3215,.F.);
#4661=ORIENTED_EDGE('',*,*,#3301,.F.);
#4662=ORIENTED_EDGE('',*,*,#3287,.F.);
#4663=ORIENTED_EDGE('',*,*,#3302,.T.);
#4664=ORIENTED_EDGE('',*,*,#3218,.F.);
#4665=ORIENTED_EDGE('',*,*,#3302,.F.);
#4666=ORIENTED_EDGE('',*,*,#3289,.F.);
#4667=ORIENTED_EDGE('',*,*,#3303,.F.);
#4668=ORIENTED_EDGE('',*,*,#3219,.F.);
#4669=ORIENTED_EDGE('',*,*,#3303,.T.);
#4670=ORIENTED_EDGE('',*,*,#3290,.F.);
#4671=ORIENTED_EDGE('',*,*,#3247,.T.);
#4672=ORIENTED_EDGE('',*,*,#3193,.F.);
#4673=ORIENTED_EDGE('',*,*,#3222,.T.);
#4674=ORIENTED_EDGE('',*,*,#3265,.F.);
#4675=ORIENTED_EDGE('',*,*,#3291,.T.);
#4676=ORIENTED_EDGE('',*,*,#3159,.F.);
#4677=ORIENTED_EDGE('',*,*,#3304,.T.);
#4678=ORIENTED_EDGE('',*,*,#3104,.F.);
#4679=ORIENTED_EDGE('',*,*,#3304,.F.);
#4680=ORIENTED_EDGE('',*,*,#3305,.F.);
#4681=ORIENTED_EDGE('',*,*,#3306,.T.);
#4682=ORIENTED_EDGE('',*,*,#3307,.F.);
#4683=ORIENTED_EDGE('',*,*,#3306,.F.);
#4684=ORIENTED_EDGE('',*,*,#3307,.T.);
#4685=ORIENTED_EDGE('',*,*,#3308,.T.);
#4686=ORIENTED_EDGE('',*,*,#3309,.T.);
#4687=ORIENTED_EDGE('',*,*,#3308,.F.);
#4688=ORIENTED_EDGE('',*,*,#3305,.T.);
#4689=ORIENTED_EDGE('',*,*,#3309,.F.);
#4690=ORIENTED_EDGE('',*,*,#3310,.T.);
#4691=ORIENTED_EDGE('',*,*,#3311,.F.);
#4692=ORIENTED_EDGE('',*,*,#3310,.F.);
#4693=ORIENTED_EDGE('',*,*,#3311,.T.);
#4694=ORIENTED_EDGE('',*,*,#3312,.F.);
#4695=ORIENTED_EDGE('',*,*,#3313,.F.);
#4696=ORIENTED_EDGE('',*,*,#3313,.T.);
#4697=ORIENTED_EDGE('',*,*,#3314,.T.);
#4698=ORIENTED_EDGE('',*,*,#3315,.T.);
#4699=ORIENTED_EDGE('',*,*,#3316,.T.);
#4700=ORIENTED_EDGE('',*,*,#3315,.F.);
#4701=ORIENTED_EDGE('',*,*,#3316,.F.);
#4702=ORIENTED_EDGE('',*,*,#3317,.T.);
#4703=ORIENTED_EDGE('',*,*,#3318,.F.);
#4704=ORIENTED_EDGE('',*,*,#3317,.F.);
#4705=ORIENTED_EDGE('',*,*,#3314,.F.);
#4706=ORIENTED_EDGE('',*,*,#3312,.T.);
#4707=ORIENTED_EDGE('',*,*,#3319,.F.);
#4708=ORIENTED_EDGE('',*,*,#3320,.T.);
#4709=ORIENTED_EDGE('',*,*,#3321,.T.);
#4710=ORIENTED_EDGE('',*,*,#3322,.F.);
#4711=ORIENTED_EDGE('',*,*,#3323,.F.);
#4712=ORIENTED_EDGE('',*,*,#3324,.T.);
#4713=ORIENTED_EDGE('',*,*,#3325,.T.);
#4714=ORIENTED_EDGE('',*,*,#3320,.F.);
#4715=ORIENTED_EDGE('',*,*,#3326,.F.);
#4716=ORIENTED_EDGE('',*,*,#3327,.T.);
#4717=ORIENTED_EDGE('',*,*,#3328,.T.);
#4718=ORIENTED_EDGE('',*,*,#3324,.F.);
#4719=ORIENTED_EDGE('',*,*,#3329,.F.);
#4720=ORIENTED_EDGE('',*,*,#3330,.T.);
#4721=ORIENTED_EDGE('',*,*,#3331,.T.);
#4722=ORIENTED_EDGE('',*,*,#3327,.F.);
#4723=ORIENTED_EDGE('',*,*,#3332,.F.);
#4724=ORIENTED_EDGE('',*,*,#3333,.T.);
#4725=ORIENTED_EDGE('',*,*,#3334,.T.);
#4726=ORIENTED_EDGE('',*,*,#3330,.F.);
#4727=ORIENTED_EDGE('',*,*,#3335,.F.);
#4728=ORIENTED_EDGE('',*,*,#3322,.T.);
#4729=ORIENTED_EDGE('',*,*,#3336,.T.);
#4730=ORIENTED_EDGE('',*,*,#3333,.F.);
#4731=ORIENTED_EDGE('',*,*,#3336,.F.);
#4732=ORIENTED_EDGE('',*,*,#3321,.F.);
#4733=ORIENTED_EDGE('',*,*,#3325,.F.);
#4734=ORIENTED_EDGE('',*,*,#3328,.F.);
#4735=ORIENTED_EDGE('',*,*,#3331,.F.);
#4736=ORIENTED_EDGE('',*,*,#3334,.F.);
#4737=ORIENTED_EDGE('',*,*,#3337,.T.);
#4738=ORIENTED_EDGE('',*,*,#3338,.T.);
#4739=ORIENTED_EDGE('',*,*,#3318,.T.);
#4740=ORIENTED_EDGE('',*,*,#3338,.F.);
#4741=ORIENTED_EDGE('',*,*,#3337,.F.);
#4742=ORIENTED_EDGE('',*,*,#3319,.T.);
#4743=ORIENTED_EDGE('',*,*,#3335,.T.);
#4744=ORIENTED_EDGE('',*,*,#3332,.T.);
#4745=ORIENTED_EDGE('',*,*,#3329,.T.);
#4746=ORIENTED_EDGE('',*,*,#3326,.T.);
#4747=ORIENTED_EDGE('',*,*,#3323,.T.);
#4748=ORIENTED_EDGE('',*,*,#3339,.T.);
#4749=ORIENTED_EDGE('',*,*,#3340,.T.);
#4750=ORIENTED_EDGE('',*,*,#3339,.F.);
#4751=ORIENTED_EDGE('',*,*,#3340,.F.);
#4752=ORIENTED_EDGE('',*,*,#3341,.F.);
#4753=ORIENTED_EDGE('',*,*,#3342,.T.);
#4754=ORIENTED_EDGE('',*,*,#3342,.F.);
#4755=ORIENTED_EDGE('',*,*,#3341,.T.);
#4756=ORIENTED_EDGE('',*,*,#3343,.T.);
#4757=ORIENTED_EDGE('',*,*,#3344,.T.);
#4758=ORIENTED_EDGE('',*,*,#3343,.F.);
#4759=ORIENTED_EDGE('',*,*,#3344,.F.);
#4760=ORIENTED_EDGE('',*,*,#3345,.F.);
#4761=ORIENTED_EDGE('',*,*,#3346,.T.);
#4762=ORIENTED_EDGE('',*,*,#3345,.T.);
#4763=ORIENTED_EDGE('',*,*,#3346,.F.);
#4764=ORIENTED_EDGE('',*,*,#3347,.T.);
#4765=ORIENTED_EDGE('',*,*,#3348,.F.);
#4766=ORIENTED_EDGE('',*,*,#3348,.T.);
#4767=ORIENTED_EDGE('',*,*,#3349,.T.);
#4768=ORIENTED_EDGE('',*,*,#3350,.F.);
#4769=ORIENTED_EDGE('',*,*,#3349,.F.);
#4770=ORIENTED_EDGE('',*,*,#3347,.F.);
#4771=ORIENTED_EDGE('',*,*,#3350,.T.);
#4772=ORIENTED_EDGE('',*,*,#3351,.F.);
#4773=ORIENTED_EDGE('',*,*,#3352,.T.);
#4774=ORIENTED_EDGE('',*,*,#3353,.F.);
#4775=ORIENTED_EDGE('',*,*,#3352,.F.);
#4776=ORIENTED_EDGE('',*,*,#3353,.T.);
#4777=ORIENTED_EDGE('',*,*,#3354,.T.);
#4778=ORIENTED_EDGE('',*,*,#3355,.T.);
#4779=ORIENTED_EDGE('',*,*,#3354,.F.);
#4780=ORIENTED_EDGE('',*,*,#3351,.T.);
#4781=ORIENTED_EDGE('',*,*,#3355,.F.);
#4782=ORIENTED_EDGE('',*,*,#3356,.T.);
#4783=ORIENTED_EDGE('',*,*,#3357,.F.);
#4784=ORIENTED_EDGE('',*,*,#3356,.F.);
#4785=ORIENTED_EDGE('',*,*,#3357,.T.);
#4786=ORIENTED_EDGE('',*,*,#3358,.T.);
#4787=ORIENTED_EDGE('',*,*,#3359,.T.);
#4788=ORIENTED_EDGE('',*,*,#3358,.F.);
#4789=ORIENTED_EDGE('',*,*,#3359,.F.);
#4790=ORIENTED_EDGE('',*,*,#3360,.F.);
#4791=ORIENTED_EDGE('',*,*,#3361,.T.);
#4792=ORIENTED_EDGE('',*,*,#3361,.F.);
#4793=ORIENTED_EDGE('',*,*,#3360,.T.);
#4794=ORIENTED_EDGE('',*,*,#3362,.T.);
#4795=ORIENTED_EDGE('',*,*,#3363,.T.);
#4796=ORIENTED_EDGE('',*,*,#3362,.F.);
#4797=ORIENTED_EDGE('',*,*,#3363,.F.);
#4798=ORIENTED_EDGE('',*,*,#3364,.T.);
#4799=ORIENTED_EDGE('',*,*,#3365,.T.);
#4800=ORIENTED_EDGE('',*,*,#3366,.T.);
#4801=ORIENTED_EDGE('',*,*,#3365,.F.);
#4802=ORIENTED_EDGE('',*,*,#3366,.F.);
#4803=ORIENTED_EDGE('',*,*,#3367,.T.);
#4804=ORIENTED_EDGE('',*,*,#3368,.F.);
#4805=ORIENTED_EDGE('',*,*,#3367,.F.);
#4806=ORIENTED_EDGE('',*,*,#3364,.F.);
#4807=ORIENTED_EDGE('',*,*,#3368,.T.);
#4808=ORIENTED_EDGE('',*,*,#3369,.T.);
#4809=ORIENTED_EDGE('',*,*,#3370,.T.);
#4810=ORIENTED_EDGE('',*,*,#3369,.F.);
#4811=ORIENTED_EDGE('',*,*,#3370,.F.);
#4812=ORIENTED_EDGE('',*,*,#3371,.F.);
#4813=ORIENTED_EDGE('',*,*,#3372,.F.);
#4814=ORIENTED_EDGE('',*,*,#3372,.T.);
#4815=ORIENTED_EDGE('',*,*,#3373,.T.);
#4816=ORIENTED_EDGE('',*,*,#3374,.T.);
#4817=ORIENTED_EDGE('',*,*,#3375,.T.);
#4818=ORIENTED_EDGE('',*,*,#3374,.F.);
#4819=ORIENTED_EDGE('',*,*,#3375,.F.);
#4820=ORIENTED_EDGE('',*,*,#3376,.T.);
#4821=ORIENTED_EDGE('',*,*,#3377,.F.);
#4822=ORIENTED_EDGE('',*,*,#3376,.F.);
#4823=ORIENTED_EDGE('',*,*,#3373,.F.);
#4824=ORIENTED_EDGE('',*,*,#3371,.T.);
#4825=ORIENTED_EDGE('',*,*,#3378,.F.);
#4826=ORIENTED_EDGE('',*,*,#3379,.T.);
#4827=ORIENTED_EDGE('',*,*,#3380,.T.);
#4828=ORIENTED_EDGE('',*,*,#3381,.F.);
#4829=ORIENTED_EDGE('',*,*,#3382,.F.);
#4830=ORIENTED_EDGE('',*,*,#3383,.T.);
#4831=ORIENTED_EDGE('',*,*,#3384,.T.);
#4832=ORIENTED_EDGE('',*,*,#3379,.F.);
#4833=ORIENTED_EDGE('',*,*,#3385,.F.);
#4834=ORIENTED_EDGE('',*,*,#3386,.T.);
#4835=ORIENTED_EDGE('',*,*,#3387,.T.);
#4836=ORIENTED_EDGE('',*,*,#3383,.F.);
#4837=ORIENTED_EDGE('',*,*,#3388,.F.);
#4838=ORIENTED_EDGE('',*,*,#3389,.T.);
#4839=ORIENTED_EDGE('',*,*,#3390,.T.);
#4840=ORIENTED_EDGE('',*,*,#3386,.F.);
#4841=ORIENTED_EDGE('',*,*,#3391,.F.);
#4842=ORIENTED_EDGE('',*,*,#3392,.T.);
#4843=ORIENTED_EDGE('',*,*,#3393,.T.);
#4844=ORIENTED_EDGE('',*,*,#3389,.F.);
#4845=ORIENTED_EDGE('',*,*,#3394,.F.);
#4846=ORIENTED_EDGE('',*,*,#3381,.T.);
#4847=ORIENTED_EDGE('',*,*,#3395,.T.);
#4848=ORIENTED_EDGE('',*,*,#3392,.F.);
#4849=ORIENTED_EDGE('',*,*,#3395,.F.);
#4850=ORIENTED_EDGE('',*,*,#3380,.F.);
#4851=ORIENTED_EDGE('',*,*,#3384,.F.);
#4852=ORIENTED_EDGE('',*,*,#3387,.F.);
#4853=ORIENTED_EDGE('',*,*,#3390,.F.);
#4854=ORIENTED_EDGE('',*,*,#3393,.F.);
#4855=ORIENTED_EDGE('',*,*,#3396,.T.);
#4856=ORIENTED_EDGE('',*,*,#3397,.T.);
#4857=ORIENTED_EDGE('',*,*,#3377,.T.);
#4858=ORIENTED_EDGE('',*,*,#3397,.F.);
#4859=ORIENTED_EDGE('',*,*,#3396,.F.);
#4860=ORIENTED_EDGE('',*,*,#3378,.T.);
#4861=ORIENTED_EDGE('',*,*,#3394,.T.);
#4862=ORIENTED_EDGE('',*,*,#3391,.T.);
#4863=ORIENTED_EDGE('',*,*,#3388,.T.);
#4864=ORIENTED_EDGE('',*,*,#3385,.T.);
#4865=ORIENTED_EDGE('',*,*,#3382,.T.);
#4866=PLANE('',#5501);
#4867=PLANE('',#5505);
#4868=PLANE('',#5509);
#4869=PLANE('',#5513);
#4870=PLANE('',#5517);
#4871=PLANE('',#5521);
#4872=PLANE('',#5525);
#4873=PLANE('',#5529);
#4874=PLANE('',#5533);
#4875=PLANE('',#5537);
#4876=PLANE('',#5541);
#4877=PLANE('',#5545);
#4878=PLANE('',#5549);
#4879=PLANE('',#5553);
#4880=PLANE('',#5557);
#4881=PLANE('',#5561);
#4882=PLANE('',#5577);
#4883=PLANE('',#5581);
#4884=PLANE('',#5585);
#4885=PLANE('',#5589);
#4886=PLANE('',#5593);
#4887=PLANE('',#5597);
#4888=PLANE('',#5601);
#4889=PLANE('',#5605);
#4890=PLANE('',#5609);
#4891=PLANE('',#5613);
#4892=PLANE('',#5617);
#4893=PLANE('',#5621);
#4894=PLANE('',#5625);
#4895=PLANE('',#5629);
#4896=PLANE('',#5633);
#4897=PLANE('',#5637);
#4898=PLANE('',#5644);
#4899=PLANE('',#5647);
#4900=PLANE('',#5650);
#4901=PLANE('',#5653);
#4902=PLANE('',#5656);
#4903=PLANE('',#5659);
#4904=PLANE('',#5662);
#4905=PLANE('',#5665);
#4906=PLANE('',#5672);
#4907=PLANE('',#5682);
#4908=PLANE('',#5685);
#4909=PLANE('',#5688);
#4910=PLANE('',#5691);
#4911=PLANE('',#5694);
#4912=PLANE('',#5697);
#4913=PLANE('',#5700);
#4914=PLANE('',#5703);
#4915=PLANE('',#5707);
#4916=PLANE('',#5711);
#4917=PLANE('',#5715);
#4918=PLANE('',#5719);
#4919=PLANE('',#5723);
#4920=PLANE('',#5727);
#4921=PLANE('',#5731);
#4922=PLANE('',#5735);
#4923=PLANE('',#5741);
#4924=PLANE('',#5743);
#4925=PLANE('',#5745);
#4926=PLANE('',#5747);
#4927=PLANE('',#5749);
#4928=PLANE('',#5751);
#4929=PLANE('',#5753);
#4930=PLANE('',#5755);
#4931=PLANE('',#5757);
#4932=PLANE('',#5761);
#4933=PLANE('',#5763);
#4934=PLANE('',#5764);
#4935=PLANE('',#5765);
#4936=PLANE('',#5785);
#4937=PLANE('',#5788);
#4938=PLANE('',#5795);
#4939=PLANE('',#5806);
#4940=PLANE('',#5807);
#4941=PLANE('',#5808);
#4942=PLANE('',#5809);
#4943=PLANE('',#5810);
#4944=PLANE('',#5811);
#4945=PLANE('',#5812);
#4946=PLANE('',#5813);
#4947=PLANE('',#5816);
#4948=PLANE('',#5821);
#4949=PLANE('',#5866);
#4950=PLANE('',#5889);
#4951=PLANE('',#5892);
#4952=PLANE('',#5895);
#4953=PLANE('',#5898);
#4954=PLANE('',#5903);
#4955=PLANE('',#5906);
#4956=PLANE('',#5909);
#4957=PLANE('',#5914);
#4958=PLANE('',#5917);
#4959=PLANE('',#5920);
#4960=PLANE('',#5923);
#4961=PLANE('',#5926);
#4962=PLANE('',#5929);
#4963=PLANE('',#5932);
#4964=PLANE('',#5935);
#4965=PLANE('',#5938);
#4966=PLANE('',#5943);
#4967=PLANE('',#5946);
#4968=PLANE('',#5949);
#4969=PLANE('',#5952);
#4970=PLANE('',#5953);
#4971=PLANE('',#5955);
#4972=PLANE('',#5957);
#4973=PLANE('',#5959);
#4974=PLANE('',#5962);
#4975=PLANE('',#5964);
#4976=PLANE('',#5966);
#4977=PLANE('',#5971);
#4978=PLANE('',#5974);
#4979=PLANE('',#5977);
#4980=PLANE('',#5980);
#4981=PLANE('',#5983);
#4982=PLANE('',#5986);
#4983=PLANE('',#5990);
#4984=PLANE('',#5992);
#4985=PLANE('',#5994);
#4986=PLANE('',#5996);
#4987=PLANE('',#5998);
#4988=PLANE('',#6000);
#4989=PLANE('',#6010);
#4990=PLANE('',#6013);
#4991=PLANE('',#6024);
#4992=PLANE('',#6025);
#4993=PLANE('',#6026);
#4994=PLANE('',#6027);
#4995=PLANE('',#6028);
#4996=PLANE('',#6029);
#4997=PLANE('',#6030);
#4998=PLANE('',#6031);
#4999=PLANE('',#6034);
#5000=PLANE('',#6041);
#5001=PLANE('',#6048);
#5002=PLANE('',#6055);
#5003=PLANE('',#6058);
#5004=PLANE('',#6065);
#5005=PLANE('',#6072);
#5006=PLANE('',#6075);
#5007=PLANE('',#6086);
#5008=PLANE('',#6087);
#5009=PLANE('',#6088);
#5010=PLANE('',#6089);
#5011=PLANE('',#6090);
#5012=PLANE('',#6091);
#5013=PLANE('',#6092);
#5014=PLANE('',#6093);
#5015=PLANE('',#6096);
#5016=ADVANCED_FACE('',(#604),#4866,.F.);
#5017=ADVANCED_FACE('',(#605),#535,.F.);
#5018=ADVANCED_FACE('',(#606),#4867,.F.);
#5019=ADVANCED_FACE('',(#607),#536,.F.);
#5020=ADVANCED_FACE('',(#608),#4868,.F.);
#5021=ADVANCED_FACE('',(#609),#537,.F.);
#5022=ADVANCED_FACE('',(#610),#4869,.F.);
#5023=ADVANCED_FACE('',(#611),#538,.F.);
#5024=ADVANCED_FACE('',(#612),#4870,.F.);
#5025=ADVANCED_FACE('',(#613),#539,.F.);
#5026=ADVANCED_FACE('',(#614),#4871,.F.);
#5027=ADVANCED_FACE('',(#615),#540,.F.);
#5028=ADVANCED_FACE('',(#616),#4872,.F.);
#5029=ADVANCED_FACE('',(#617),#541,.F.);
#5030=ADVANCED_FACE('',(#618),#4873,.F.);
#5031=ADVANCED_FACE('',(#619),#542,.F.);
#5032=ADVANCED_FACE('',(#620),#4874,.F.);
#5033=ADVANCED_FACE('',(#621),#543,.F.);
#5034=ADVANCED_FACE('',(#622),#4875,.F.);
#5035=ADVANCED_FACE('',(#623),#544,.F.);
#5036=ADVANCED_FACE('',(#624),#4876,.F.);
#5037=ADVANCED_FACE('',(#625),#545,.F.);
#5038=ADVANCED_FACE('',(#626),#4877,.F.);
#5039=ADVANCED_FACE('',(#627),#546,.F.);
#5040=ADVANCED_FACE('',(#628),#4878,.F.);
#5041=ADVANCED_FACE('',(#629),#547,.F.);
#5042=ADVANCED_FACE('',(#630),#4879,.F.);
#5043=ADVANCED_FACE('',(#631),#548,.F.);
#5044=ADVANCED_FACE('',(#632),#4880,.F.);
#5045=ADVANCED_FACE('',(#633),#549,.F.);
#5046=ADVANCED_FACE('',(#634),#4881,.F.);
#5047=ADVANCED_FACE('',(#635),#550,.F.);
#5048=ADVANCED_FACE('',(#636),#551,.F.);
#5049=ADVANCED_FACE('',(#637),#552,.F.);
#5050=ADVANCED_FACE('',(#638),#183,.F.);
#5051=ADVANCED_FACE('',(#639),#184,.T.);
#5052=ADVANCED_FACE('',(#640),#4882,.T.);
#5053=ADVANCED_FACE('',(#641),#185,.T.);
#5054=ADVANCED_FACE('',(#642),#4883,.T.);
#5055=ADVANCED_FACE('',(#643),#186,.T.);
#5056=ADVANCED_FACE('',(#644),#4884,.T.);
#5057=ADVANCED_FACE('',(#645),#187,.T.);
#5058=ADVANCED_FACE('',(#646),#4885,.T.);
#5059=ADVANCED_FACE('',(#647),#188,.T.);
#5060=ADVANCED_FACE('',(#648),#4886,.T.);
#5061=ADVANCED_FACE('',(#649),#189,.T.);
#5062=ADVANCED_FACE('',(#650),#4887,.T.);
#5063=ADVANCED_FACE('',(#651),#190,.T.);
#5064=ADVANCED_FACE('',(#652),#4888,.T.);
#5065=ADVANCED_FACE('',(#653),#191,.T.);
#5066=ADVANCED_FACE('',(#654),#4889,.T.);
#5067=ADVANCED_FACE('',(#655),#192,.T.);
#5068=ADVANCED_FACE('',(#656),#4890,.T.);
#5069=ADVANCED_FACE('',(#657),#193,.T.);
#5070=ADVANCED_FACE('',(#658),#4891,.T.);
#5071=ADVANCED_FACE('',(#659),#194,.T.);
#5072=ADVANCED_FACE('',(#660),#4892,.T.);
#5073=ADVANCED_FACE('',(#661),#195,.T.);
#5074=ADVANCED_FACE('',(#662),#4893,.T.);
#5075=ADVANCED_FACE('',(#663),#196,.T.);
#5076=ADVANCED_FACE('',(#664),#4894,.T.);
#5077=ADVANCED_FACE('',(#665),#197,.T.);
#5078=ADVANCED_FACE('',(#666),#4895,.T.);
#5079=ADVANCED_FACE('',(#667),#198,.T.);
#5080=ADVANCED_FACE('',(#668),#4896,.T.);
#5081=ADVANCED_FACE('',(#669),#199,.T.);
#5082=ADVANCED_FACE('',(#670),#4897,.T.);
#5083=ADVANCED_FACE('',(#671),#200,.T.);
#5084=ADVANCED_FACE('',(#672),#201,.F.);
#5085=ADVANCED_FACE('',(#673),#4898,.T.);
#5086=ADVANCED_FACE('',(#674),#553,.T.);
#5087=ADVANCED_FACE('',(#675),#4899,.T.);
#5088=ADVANCED_FACE('',(#676),#554,.T.);
#5089=ADVANCED_FACE('',(#677),#4900,.T.);
#5090=ADVANCED_FACE('',(#678),#555,.T.);
#5091=ADVANCED_FACE('',(#679),#4901,.T.);
#5092=ADVANCED_FACE('',(#680),#556,.T.);
#5093=ADVANCED_FACE('',(#681),#4902,.T.);
#5094=ADVANCED_FACE('',(#682),#557,.T.);
#5095=ADVANCED_FACE('',(#683),#4903,.T.);
#5096=ADVANCED_FACE('',(#684),#558,.T.);
#5097=ADVANCED_FACE('',(#685),#4904,.T.);
#5098=ADVANCED_FACE('',(#686),#559,.T.);
#5099=ADVANCED_FACE('',(#687),#4905,.T.);
#5100=ADVANCED_FACE('',(#688),#560,.T.);
#5101=ADVANCED_FACE('',(#689),#561,.F.);
#5102=ADVANCED_FACE('',(#690),#562,.F.);
#5103=ADVANCED_FACE('',(#691,#132,#133,#134,#135,#136,#137,#138),#4906,
 .T.);
#5104=ADVANCED_FACE('',(#692),#202,.F.);
#5105=ADVANCED_FACE('',(#693),#203,.T.);
#5106=ADVANCED_FACE('',(#694),#4907,.T.);
#5107=ADVANCED_FACE('',(#695),#204,.T.);
#5108=ADVANCED_FACE('',(#696),#4908,.T.);
#5109=ADVANCED_FACE('',(#697),#205,.T.);
#5110=ADVANCED_FACE('',(#698),#4909,.T.);
#5111=ADVANCED_FACE('',(#699),#206,.T.);
#5112=ADVANCED_FACE('',(#700),#4910,.T.);
#5113=ADVANCED_FACE('',(#701),#207,.T.);
#5114=ADVANCED_FACE('',(#702),#4911,.T.);
#5115=ADVANCED_FACE('',(#703),#208,.T.);
#5116=ADVANCED_FACE('',(#704),#4912,.T.);
#5117=ADVANCED_FACE('',(#705),#209,.T.);
#5118=ADVANCED_FACE('',(#706),#4913,.T.);
#5119=ADVANCED_FACE('',(#707),#210,.T.);
#5120=ADVANCED_FACE('',(#708),#4914,.T.);
#5121=ADVANCED_FACE('',(#709),#211,.T.);
#5122=ADVANCED_FACE('',(#710),#4915,.T.);
#5123=ADVANCED_FACE('',(#711),#212,.T.);
#5124=ADVANCED_FACE('',(#712),#4916,.T.);
#5125=ADVANCED_FACE('',(#713),#213,.T.);
#5126=ADVANCED_FACE('',(#714),#4917,.T.);
#5127=ADVANCED_FACE('',(#715),#214,.T.);
#5128=ADVANCED_FACE('',(#716),#4918,.T.);
#5129=ADVANCED_FACE('',(#717),#215,.T.);
#5130=ADVANCED_FACE('',(#718),#4919,.T.);
#5131=ADVANCED_FACE('',(#719),#216,.T.);
#5132=ADVANCED_FACE('',(#720),#4920,.T.);
#5133=ADVANCED_FACE('',(#721),#217,.T.);
#5134=ADVANCED_FACE('',(#722),#4921,.T.);
#5135=ADVANCED_FACE('',(#723),#218,.T.);
#5136=ADVANCED_FACE('',(#724),#4922,.T.);
#5137=ADVANCED_FACE('',(#725),#219,.T.);
#5138=ADVANCED_FACE('',(#726),#220,.F.);
#5139=ADVANCED_FACE('',(#727),#4923,.F.);
#5140=ADVANCED_FACE('',(#728),#563,.T.);
#5141=ADVANCED_FACE('',(#729),#4924,.F.);
#5142=ADVANCED_FACE('',(#730),#564,.T.);
#5143=ADVANCED_FACE('',(#731),#4925,.F.);
#5144=ADVANCED_FACE('',(#732),#565,.T.);
#5145=ADVANCED_FACE('',(#733),#4926,.F.);
#5146=ADVANCED_FACE('',(#734),#566,.T.);
#5147=ADVANCED_FACE('',(#735),#4927,.F.);
#5148=ADVANCED_FACE('',(#736),#567,.T.);
#5149=ADVANCED_FACE('',(#737),#4928,.F.);
#5150=ADVANCED_FACE('',(#738),#568,.T.);
#5151=ADVANCED_FACE('',(#739),#4929,.F.);
#5152=ADVANCED_FACE('',(#740),#569,.T.);
#5153=ADVANCED_FACE('',(#741),#4930,.F.);
#5154=ADVANCED_FACE('',(#742),#570,.T.);
#5155=ADVANCED_FACE('',(#743,#139,#140,#141,#142,#143,#144,#145),#4931,
 .F.);
#5156=ADVANCED_FACE('',(#744,#146),#4932,.T.);
#5157=ADVANCED_FACE('',(#745,#147),#4933,.T.);
#5158=ADVANCED_FACE('',(#746,#148),#4934,.T.);
#5159=ADVANCED_FACE('',(#747,#149),#4935,.T.);
#5160=ADVANCED_FACE('',(#748),#221,.F.);
#5161=ADVANCED_FACE('',(#749),#571,.F.);
#5162=ADVANCED_FACE('',(#750),#222,.F.);
#5163=ADVANCED_FACE('',(#751),#572,.F.);
#5164=ADVANCED_FACE('',(#752),#223,.F.);
#5165=ADVANCED_FACE('',(#753),#573,.F.);
#5166=ADVANCED_FACE('',(#754),#574,.F.);
#5167=ADVANCED_FACE('',(#755),#575,.F.);
#5168=ADVANCED_FACE('',(#756),#576,.T.);
#5169=ADVANCED_FACE('',(#757),#224,.T.);
#5170=ADVANCED_FACE('',(#758),#577,.T.);
#5171=ADVANCED_FACE('',(#759),#4936,.T.);
#5172=ADVANCED_FACE('',(#760),#225,.T.);
#5173=ADVANCED_FACE('',(#761),#4937,.F.);
#5174=ADVANCED_FACE('',(#762,#150),#73,.T.);
#5175=ADVANCED_FACE('',(#763),#69,.T.);
#5176=ADVANCED_FACE('',(#764),#4938,.T.);
#5177=ADVANCED_FACE('',(#765),#63,.T.);
#5178=ADVANCED_FACE('',(#766),#74,.T.);
#5179=ADVANCED_FACE('',(#767),#578,.T.);
#5180=ADVANCED_FACE('',(#768,#151),#4939,.F.);
#5181=ADVANCED_FACE('',(#769),#4940,.F.);
#5182=ADVANCED_FACE('',(#770),#4941,.F.);
#5183=ADVANCED_FACE('',(#771),#4942,.F.);
#5184=ADVANCED_FACE('',(#772),#4943,.F.);
#5185=ADVANCED_FACE('',(#773),#4944,.F.);
#5186=ADVANCED_FACE('',(#774),#4945,.F.);
#5187=ADVANCED_FACE('',(#775),#4946,.F.);
#5188=ADVANCED_FACE('',(#776),#226,.T.);
#5189=ADVANCED_FACE('',(#777,#152),#4947,.T.);
#5190=ADVANCED_FACE('',(#778),#64,.F.);
#5191=ADVANCED_FACE('',(#779,#153,#154,#155,#156,#157,#158,#159,#160),#4948,
 .F.);
#5192=ADVANCED_FACE('',(#780),#65,.F.);
#5193=ADVANCED_FACE('',(#781),#66,.F.);
#5194=ADVANCED_FACE('',(#782),#227,.F.);
#5195=ADVANCED_FACE('',(#783),#579,.F.);
#5196=ADVANCED_FACE('',(#784),#228,.F.);
#5197=ADVANCED_FACE('',(#785),#580,.F.);
#5198=ADVANCED_FACE('',(#786),#229,.F.);
#5199=ADVANCED_FACE('',(#787),#581,.F.);
#5200=ADVANCED_FACE('',(#788),#230,.F.);
#5201=ADVANCED_FACE('',(#789),#582,.F.);
#5202=ADVANCED_FACE('',(#790),#231,.F.);
#5203=ADVANCED_FACE('',(#791,#161,#162,#163,#164,#165),#4949,.T.);
#5204=ADVANCED_FACE('',(#792),#232,.F.);
#5205=ADVANCED_FACE('',(#793),#233,.F.);
#5206=ADVANCED_FACE('',(#794),#234,.F.);
#5207=ADVANCED_FACE('',(#795),#4950,.T.);
#5208=ADVANCED_FACE('',(#796),#235,.T.);
#5209=ADVANCED_FACE('',(#797),#4951,.T.);
#5210=ADVANCED_FACE('',(#798),#236,.T.);
#5211=ADVANCED_FACE('',(#799),#4952,.T.);
#5212=ADVANCED_FACE('',(#800),#237,.T.);
#5213=ADVANCED_FACE('',(#801),#4953,.T.);
#5214=ADVANCED_FACE('',(#802),#238,.F.);
#5215=ADVANCED_FACE('',(#803),#239,.T.);
#5216=ADVANCED_FACE('',(#804),#4954,.T.);
#5217=ADVANCED_FACE('',(#805),#240,.T.);
#5218=ADVANCED_FACE('',(#806),#4955,.T.);
#5219=ADVANCED_FACE('',(#807),#241,.T.);
#5220=ADVANCED_FACE('',(#808),#4956,.T.);
#5221=ADVANCED_FACE('',(#809),#242,.T.);
#5222=ADVANCED_FACE('',(#810),#243,.F.);
#5223=ADVANCED_FACE('',(#811),#4957,.T.);
#5224=ADVANCED_FACE('',(#812),#244,.T.);
#5225=ADVANCED_FACE('',(#813),#4958,.T.);
#5226=ADVANCED_FACE('',(#814),#245,.T.);
#5227=ADVANCED_FACE('',(#815),#4959,.T.);
#5228=ADVANCED_FACE('',(#816),#246,.T.);
#5229=ADVANCED_FACE('',(#817),#4960,.T.);
#5230=ADVANCED_FACE('',(#818),#247,.T.);
#5231=ADVANCED_FACE('',(#819),#4961,.T.);
#5232=ADVANCED_FACE('',(#820),#248,.T.);
#5233=ADVANCED_FACE('',(#821),#4962,.T.);
#5234=ADVANCED_FACE('',(#822),#249,.T.);
#5235=ADVANCED_FACE('',(#823),#4963,.F.);
#5236=ADVANCED_FACE('',(#824),#583,.T.);
#5237=ADVANCED_FACE('',(#825),#4964,.T.);
#5238=ADVANCED_FACE('',(#826),#584,.T.);
#5239=ADVANCED_FACE('',(#827),#4965,.T.);
#5240=ADVANCED_FACE('',(#828),#585,.T.);
#5241=ADVANCED_FACE('',(#829),#586,.F.);
#5242=ADVANCED_FACE('',(#830),#4966,.T.);
#5243=ADVANCED_FACE('',(#831),#587,.T.);
#5244=ADVANCED_FACE('',(#832),#4967,.T.);
#5245=ADVANCED_FACE('',(#833),#588,.T.);
#5246=ADVANCED_FACE('',(#834),#4968,.T.);
#5247=ADVANCED_FACE('',(#835),#589,.T.);
#5248=ADVANCED_FACE('',(#836),#4969,.T.);
#5249=ADVANCED_FACE('',(#837),#4970,.T.);
#5250=ADVANCED_FACE('',(#838),#250,.T.);
#5251=ADVANCED_FACE('',(#839),#4971,.T.);
#5252=ADVANCED_FACE('',(#840),#251,.T.);
#5253=ADVANCED_FACE('',(#841),#4972,.T.);
#5254=ADVANCED_FACE('',(#842),#252,.T.);
#5255=ADVANCED_FACE('',(#843),#4973,.T.);
#5256=ADVANCED_FACE('',(#844),#253,.F.);
#5257=ADVANCED_FACE('',(#845),#254,.T.);
#5258=ADVANCED_FACE('',(#846),#4974,.T.);
#5259=ADVANCED_FACE('',(#847),#255,.T.);
#5260=ADVANCED_FACE('',(#848),#4975,.T.);
#5261=ADVANCED_FACE('',(#849),#256,.T.);
#5262=ADVANCED_FACE('',(#850),#4976,.T.);
#5263=ADVANCED_FACE('',(#851),#257,.T.);
#5264=ADVANCED_FACE('',(#852),#258,.F.);
#5265=ADVANCED_FACE('',(#853),#4977,.T.);
#5266=ADVANCED_FACE('',(#854),#259,.T.);
#5267=ADVANCED_FACE('',(#855),#4978,.T.);
#5268=ADVANCED_FACE('',(#856),#260,.T.);
#5269=ADVANCED_FACE('',(#857),#4979,.T.);
#5270=ADVANCED_FACE('',(#858),#261,.T.);
#5271=ADVANCED_FACE('',(#859),#4980,.T.);
#5272=ADVANCED_FACE('',(#860),#262,.T.);
#5273=ADVANCED_FACE('',(#861),#4981,.T.);
#5274=ADVANCED_FACE('',(#862),#263,.T.);
#5275=ADVANCED_FACE('',(#863),#4982,.T.);
#5276=ADVANCED_FACE('',(#864),#264,.T.);
#5277=ADVANCED_FACE('',(#865),#590,.F.);
#5278=ADVANCED_FACE('',(#866),#4983,.F.);
#5279=ADVANCED_FACE('',(#867),#591,.T.);
#5280=ADVANCED_FACE('',(#868),#4984,.F.);
#5281=ADVANCED_FACE('',(#869),#592,.T.);
#5282=ADVANCED_FACE('',(#870),#4985,.F.);
#5283=ADVANCED_FACE('',(#871),#593,.T.);
#5284=ADVANCED_FACE('',(#872),#4986,.F.);
#5285=ADVANCED_FACE('',(#873),#594,.T.);
#5286=ADVANCED_FACE('',(#874),#4987,.F.);
#5287=ADVANCED_FACE('',(#875),#595,.T.);
#5288=ADVANCED_FACE('',(#876),#4988,.T.);
#5289=ADVANCED_FACE('',(#877),#596,.T.);
#5290=ADVANCED_FACE('',(#878),#597,.T.);
#5291=ADVANCED_FACE('',(#879),#598,.F.);
#5292=ADVANCED_FACE('',(#880),#265,.T.);
#5293=ADVANCED_FACE('',(#881),#599,.T.);
#5294=ADVANCED_FACE('',(#882),#4989,.F.);
#5295=ADVANCED_FACE('',(#883),#266,.T.);
#5296=ADVANCED_FACE('',(#884),#4990,.T.);
#5297=ADVANCED_FACE('',(#885),#67,.T.);
#5298=ADVANCED_FACE('',(#886),#75,.T.);
#5299=ADVANCED_FACE('',(#887),#600,.T.);
#5300=ADVANCED_FACE('',(#888,#166),#4991,.F.);
#5301=ADVANCED_FACE('',(#889),#4992,.F.);
#5302=ADVANCED_FACE('',(#890),#4993,.F.);
#5303=ADVANCED_FACE('',(#891),#4994,.F.);
#5304=ADVANCED_FACE('',(#892),#4995,.F.);
#5305=ADVANCED_FACE('',(#893),#4996,.F.);
#5306=ADVANCED_FACE('',(#894),#4997,.F.);
#5307=ADVANCED_FACE('',(#895),#4998,.F.);
#5308=ADVANCED_FACE('',(#896),#267,.T.);
#5309=ADVANCED_FACE('',(#897,#167),#4999,.T.);
#5310=ADVANCED_FACE('',(#898,#168),#76,.T.);
#5311=ADVANCED_FACE('',(#899),#70,.F.);
#5312=ADVANCED_FACE('',(#900),#5000,.F.);
#5313=ADVANCED_FACE('',(#901,#169),#77,.T.);
#5314=ADVANCED_FACE('',(#902),#71,.T.);
#5315=ADVANCED_FACE('',(#903),#5001,.T.);
#5316=ADVANCED_FACE('',(#904),#268,.T.);
#5317=ADVANCED_FACE('',(#905),#601,.T.);
#5318=ADVANCED_FACE('',(#906),#5002,.F.);
#5319=ADVANCED_FACE('',(#907),#269,.T.);
#5320=ADVANCED_FACE('',(#908),#5003,.T.);
#5321=ADVANCED_FACE('',(#909,#170),#78,.T.);
#5322=ADVANCED_FACE('',(#910),#72,.F.);
#5323=ADVANCED_FACE('',(#911),#5004,.F.);
#5324=ADVANCED_FACE('',(#912),#270,.T.);
#5325=ADVANCED_FACE('',(#913),#602,.T.);
#5326=ADVANCED_FACE('',(#914),#5005,.T.);
#5327=ADVANCED_FACE('',(#915),#271,.T.);
#5328=ADVANCED_FACE('',(#916),#5006,.F.);
#5329=ADVANCED_FACE('',(#917),#68,.T.);
#5330=ADVANCED_FACE('',(#918),#79,.T.);
#5331=ADVANCED_FACE('',(#919),#603,.T.);
#5332=ADVANCED_FACE('',(#920,#171),#5007,.F.);
#5333=ADVANCED_FACE('',(#921),#5008,.F.);
#5334=ADVANCED_FACE('',(#922),#5009,.F.);
#5335=ADVANCED_FACE('',(#923),#5010,.F.);
#5336=ADVANCED_FACE('',(#924),#5011,.F.);
#5337=ADVANCED_FACE('',(#925),#5012,.F.);
#5338=ADVANCED_FACE('',(#926),#5013,.F.);
#5339=ADVANCED_FACE('',(#927),#5014,.F.);
#5340=ADVANCED_FACE('',(#928),#272,.T.);
#5341=ADVANCED_FACE('',(#929,#172),#5015,.T.);
#5342=CLOSED_SHELL('',(#5016,#5017,#5018,#5019,#5020,#5021,#5022,#5023,
#5024,#5025,#5026,#5027,#5028,#5029,#5030,#5031,#5032,#5033,#5034,#5035,
#5036,#5037,#5038,#5039,#5040,#5041,#5042,#5043,#5044,#5045,#5046,#5047,
#5048,#5049,#5050,#5051,#5052,#5053,#5054,#5055,#5056,#5057,#5058,#5059,
#5060,#5061,#5062,#5063,#5064,#5065,#5066,#5067,#5068,#5069,#5070,#5071,
#5072,#5073,#5074,#5075,#5076,#5077,#5078,#5079,#5080,#5081,#5082,#5083,
#5084,#5085,#5086,#5087,#5088,#5089,#5090,#5091,#5092,#5093,#5094,#5095,
#5096,#5097,#5098,#5099,#5100,#5101,#5102,#5103,#5104,#5105,#5106,#5107,
#5108,#5109,#5110,#5111,#5112,#5113,#5114,#5115,#5116,#5117,#5118,#5119,
#5120,#5121,#5122,#5123,#5124,#5125,#5126,#5127,#5128,#5129,#5130,#5131,
#5132,#5133,#5134,#5135,#5136,#5137,#5138,#5139,#5140,#5141,#5142,#5143,
#5144,#5145,#5146,#5147,#5148,#5149,#5150,#5151,#5152,#5153,#5154,#5155,
#5156,#5157,#5158,#5159,#5160,#5161,#5162,#5163,#5164,#5165,#5166,#5167,
#5168));
#5343=CLOSED_SHELL('',(#5169,#5170,#5171,#5172,#5173));
#5344=CLOSED_SHELL('',(#5174,#5175,#5176));
#5345=CLOSED_SHELL('',(#5177,#5178,#5179,#5180,#5181,#5182,#5183,#5184,
#5185,#5186,#5187,#5188,#5189));
#5346=CLOSED_SHELL('',(#5190,#5191,#5192,#5193,#5194,#5195,#5196,#5197,
#5198,#5199,#5200,#5201,#5202,#5203,#5204,#5205,#5206,#5207,#5208,#5209,
#5210,#5211,#5212,#5213,#5214,#5215,#5216,#5217,#5218,#5219,#5220,#5221,
#5222,#5223,#5224,#5225,#5226,#5227,#5228,#5229,#5230,#5231,#5232,#5233,
#5234,#5235,#5236,#5237,#5238,#5239,#5240,#5241,#5242,#5243,#5244,#5245,
#5246,#5247,#5248,#5249,#5250,#5251,#5252,#5253,#5254,#5255,#5256,#5257,
#5258,#5259,#5260,#5261,#5262,#5263,#5264,#5265,#5266,#5267,#5268,#5269,
#5270,#5271,#5272,#5273,#5274,#5275,#5276,#5277,#5278,#5279,#5280,#5281,
#5282,#5283,#5284,#5285,#5286,#5287,#5288,#5289,#5290,#5291));
#5347=CLOSED_SHELL('',(#5292,#5293,#5294,#5295,#5296));
#5348=CLOSED_SHELL('',(#5297,#5298,#5299,#5300,#5301,#5302,#5303,#5304,
#5305,#5306,#5307,#5308,#5309));
#5349=CLOSED_SHELL('',(#5310,#5311,#5312));
#5350=CLOSED_SHELL('',(#5313,#5314,#5315));
#5351=CLOSED_SHELL('',(#5316,#5317,#5318,#5319,#5320));
#5352=CLOSED_SHELL('',(#5321,#5322,#5323));
#5353=CLOSED_SHELL('',(#5324,#5325,#5326,#5327,#5328));
#5354=CLOSED_SHELL('',(#5329,#5330,#5331,#5332,#5333,#5334,#5335,#5336,
#5337,#5338,#5339,#5340,#5341));
#5355=DERIVED_UNIT_ELEMENT(#5381,1.);
#5356=DERIVED_UNIT_ELEMENT(#11387,-3.);
#5357=DERIVED_UNIT_ELEMENT(#5381,1.);
#5358=DERIVED_UNIT_ELEMENT(#11387,-3.);
#5359=DERIVED_UNIT_ELEMENT(#5381,1.);
#5360=DERIVED_UNIT_ELEMENT(#11387,-3.);
#5361=DERIVED_UNIT_ELEMENT(#5381,1.);
#5362=DERIVED_UNIT_ELEMENT(#11387,-3.);
#5363=DERIVED_UNIT_ELEMENT(#5381,1.);
#5364=DERIVED_UNIT_ELEMENT(#11387,-3.);
#5365=DERIVED_UNIT_ELEMENT(#5381,1.);
#5366=DERIVED_UNIT_ELEMENT(#11387,-3.);
#5367=DERIVED_UNIT_ELEMENT(#5381,1.);
#5368=DERIVED_UNIT_ELEMENT(#11387,-3.);
#5369=DERIVED_UNIT_ELEMENT(#5381,1.);
#5370=DERIVED_UNIT_ELEMENT(#11387,-3.);
#5371=DERIVED_UNIT_ELEMENT(#5381,1.);
#5372=DERIVED_UNIT_ELEMENT(#11387,-3.);
#5373=DERIVED_UNIT_ELEMENT(#5381,1.);
#5374=DERIVED_UNIT_ELEMENT(#11387,-3.);
#5375=DERIVED_UNIT_ELEMENT(#5381,1.);
#5376=DERIVED_UNIT_ELEMENT(#11387,-3.);
#5377=DERIVED_UNIT_ELEMENT(#5381,1.);
#5378=DERIVED_UNIT_ELEMENT(#11387,-3.);
#5379=DERIVED_UNIT_ELEMENT(#5381,1.);
#5380=DERIVED_UNIT_ELEMENT(#11387,-3.);
#5381=(
MASS_UNIT()
NAMED_UNIT(*)
SI_UNIT(.KILO.,.GRAM.)
);
#5382=DERIVED_UNIT((#5355,#5356));
#5383=DERIVED_UNIT((#5357,#5358));
#5384=DERIVED_UNIT((#5359,#5360));
#5385=DERIVED_UNIT((#5361,#5362));
#5386=DERIVED_UNIT((#5363,#5364));
#5387=DERIVED_UNIT((#5365,#5366));
#5388=DERIVED_UNIT((#5367,#5368));
#5389=DERIVED_UNIT((#5369,#5370));
#5390=DERIVED_UNIT((#5371,#5372));
#5391=DERIVED_UNIT((#5373,#5374));
#5392=DERIVED_UNIT((#5375,#5376));
#5393=DERIVED_UNIT((#5377,#5378));
#5394=DERIVED_UNIT((#5379,#5380));
#5395=MEASURE_REPRESENTATION_ITEM('density measure',
POSITIVE_RATIO_MEASURE(7850.),#5382);
#5396=MEASURE_REPRESENTATION_ITEM('density measure',
POSITIVE_RATIO_MEASURE(7850.),#5383);
#5397=MEASURE_REPRESENTATION_ITEM('density measure',
POSITIVE_RATIO_MEASURE(7850.),#5384);
#5398=MEASURE_REPRESENTATION_ITEM('density measure',
POSITIVE_RATIO_MEASURE(7850.),#5385);
#5399=MEASURE_REPRESENTATION_ITEM('density measure',
POSITIVE_RATIO_MEASURE(7850.),#5386);
#5400=MEASURE_REPRESENTATION_ITEM('density measure',
POSITIVE_RATIO_MEASURE(7850.),#5387);
#5401=MEASURE_REPRESENTATION_ITEM('density measure',
POSITIVE_RATIO_MEASURE(7850.),#5388);
#5402=MEASURE_REPRESENTATION_ITEM('density measure',
POSITIVE_RATIO_MEASURE(7850.),#5389);
#5403=MEASURE_REPRESENTATION_ITEM('density measure',
POSITIVE_RATIO_MEASURE(7850.),#5390);
#5404=MEASURE_REPRESENTATION_ITEM('density measure',
POSITIVE_RATIO_MEASURE(7850.),#5391);
#5405=MEASURE_REPRESENTATION_ITEM('density measure',
POSITIVE_RATIO_MEASURE(7850.),#5392);
#5406=MEASURE_REPRESENTATION_ITEM('density measure',
POSITIVE_RATIO_MEASURE(7850.),#5393);
#5407=MEASURE_REPRESENTATION_ITEM('density measure',
POSITIVE_RATIO_MEASURE(7850.),#5394);
#5408=PROPERTY_DEFINITION_REPRESENTATION(#5473,#5434);
#5409=PROPERTY_DEFINITION_REPRESENTATION(#5474,#5435);
#5410=PROPERTY_DEFINITION_REPRESENTATION(#5475,#5436);
#5411=PROPERTY_DEFINITION_REPRESENTATION(#5476,#5437);
#5412=PROPERTY_DEFINITION_REPRESENTATION(#5477,#5438);
#5413=PROPERTY_DEFINITION_REPRESENTATION(#5478,#5439);
#5414=PROPERTY_DEFINITION_REPRESENTATION(#5479,#5440);
#5415=PROPERTY_DEFINITION_REPRESENTATION(#5480,#5441);
#5416=PROPERTY_DEFINITION_REPRESENTATION(#5481,#5442);
#5417=PROPERTY_DEFINITION_REPRESENTATION(#5482,#5443);
#5418=PROPERTY_DEFINITION_REPRESENTATION(#5483,#5444);
#5419=PROPERTY_DEFINITION_REPRESENTATION(#5484,#5445);
#5420=PROPERTY_DEFINITION_REPRESENTATION(#5485,#5446);
#5421=PROPERTY_DEFINITION_REPRESENTATION(#5486,#5447);
#5422=PROPERTY_DEFINITION_REPRESENTATION(#5487,#5448);
#5423=PROPERTY_DEFINITION_REPRESENTATION(#5488,#5449);
#5424=PROPERTY_DEFINITION_REPRESENTATION(#5489,#5450);
#5425=PROPERTY_DEFINITION_REPRESENTATION(#5490,#5451);
#5426=PROPERTY_DEFINITION_REPRESENTATION(#5491,#5452);
#5427=PROPERTY_DEFINITION_REPRESENTATION(#5492,#5453);
#5428=PROPERTY_DEFINITION_REPRESENTATION(#5493,#5454);
#5429=PROPERTY_DEFINITION_REPRESENTATION(#5494,#5455);
#5430=PROPERTY_DEFINITION_REPRESENTATION(#5495,#5456);
#5431=PROPERTY_DEFINITION_REPRESENTATION(#5496,#5457);
#5432=PROPERTY_DEFINITION_REPRESENTATION(#5497,#5458);
#5433=PROPERTY_DEFINITION_REPRESENTATION(#5498,#5459);
#5434=REPRESENTATION('material name',(#5460),#11372);
#5435=REPRESENTATION('density',(#5395),#11372);
#5436=REPRESENTATION('material name',(#5461),#11373);
#5437=REPRESENTATION('density',(#5396),#11373);
#5438=REPRESENTATION('material name',(#5462),#11374);
#5439=REPRESENTATION('density',(#5397),#11374);
#5440=REPRESENTATION('material name',(#5463),#11375);
#5441=REPRESENTATION('density',(#5398),#11375);
#5442=REPRESENTATION('material name',(#5464),#11376);
#5443=REPRESENTATION('density',(#5399),#11376);
#5444=REPRESENTATION('material name',(#5465),#11377);
#5445=REPRESENTATION('density',(#5400),#11377);
#5446=REPRESENTATION('material name',(#5466),#11378);
#5447=REPRESENTATION('density',(#5401),#11378);
#5448=REPRESENTATION('material name',(#5467),#11379);
#5449=REPRESENTATION('density',(#5402),#11379);
#5450=REPRESENTATION('material name',(#5468),#11380);
#5451=REPRESENTATION('density',(#5403),#11380);
#5452=REPRESENTATION('material name',(#5469),#11381);
#5453=REPRESENTATION('density',(#5404),#11381);
#5454=REPRESENTATION('material name',(#5470),#11382);
#5455=REPRESENTATION('density',(#5405),#11382);
#5456=REPRESENTATION('material name',(#5471),#11383);
#5457=REPRESENTATION('density',(#5406),#11383);
#5458=REPRESENTATION('material name',(#5472),#11384);
#5459=REPRESENTATION('density',(#5407),#11384);
#5460=DESCRIPTIVE_REPRESENTATION_ITEM('Steel','Steel');
#5461=DESCRIPTIVE_REPRESENTATION_ITEM('Steel','Steel');
#5462=DESCRIPTIVE_REPRESENTATION_ITEM('Steel','Steel');
#5463=DESCRIPTIVE_REPRESENTATION_ITEM('Steel','Steel');
#5464=DESCRIPTIVE_REPRESENTATION_ITEM('Steel','Steel');
#5465=DESCRIPTIVE_REPRESENTATION_ITEM('Steel','Steel');
#5466=DESCRIPTIVE_REPRESENTATION_ITEM('Steel','Steel');
#5467=DESCRIPTIVE_REPRESENTATION_ITEM('Steel','Steel');
#5468=DESCRIPTIVE_REPRESENTATION_ITEM('Steel','Steel');
#5469=DESCRIPTIVE_REPRESENTATION_ITEM('Steel','Steel');
#5470=DESCRIPTIVE_REPRESENTATION_ITEM('Steel','Steel');
#5471=DESCRIPTIVE_REPRESENTATION_ITEM('Steel','Steel');
#5472=DESCRIPTIVE_REPRESENTATION_ITEM('Steel','Steel');
#5473=PROPERTY_DEFINITION('material property','material name',#11447);
#5474=PROPERTY_DEFINITION('material property','density of part',#11447);
#5475=PROPERTY_DEFINITION('material property','material name',#11448);
#5476=PROPERTY_DEFINITION('material property','density of part',#11448);
#5477=PROPERTY_DEFINITION('material property','material name',#11449);
#5478=PROPERTY_DEFINITION('material property','density of part',#11449);
#5479=PROPERTY_DEFINITION('material property','material name',#11450);
#5480=PROPERTY_DEFINITION('material property','density of part',#11450);
#5481=PROPERTY_DEFINITION('material property','material name',#11451);
#5482=PROPERTY_DEFINITION('material property','density of part',#11451);
#5483=PROPERTY_DEFINITION('material property','material name',#11452);
#5484=PROPERTY_DEFINITION('material property','density of part',#11452);
#5485=PROPERTY_DEFINITION('material property','material name',#11453);
#5486=PROPERTY_DEFINITION('material property','density of part',#11453);
#5487=PROPERTY_DEFINITION('material property','material name',#11454);
#5488=PROPERTY_DEFINITION('material property','density of part',#11454);
#5489=PROPERTY_DEFINITION('material property','material name',#11455);
#5490=PROPERTY_DEFINITION('material property','density of part',#11455);
#5491=PROPERTY_DEFINITION('material property','material name',#11456);
#5492=PROPERTY_DEFINITION('material property','density of part',#11456);
#5493=PROPERTY_DEFINITION('material property','material name',#11457);
#5494=PROPERTY_DEFINITION('material property','density of part',#11457);
#5495=PROPERTY_DEFINITION('material property','material name',#11458);
#5496=PROPERTY_DEFINITION('material property','density of part',#11458);
#5497=PROPERTY_DEFINITION('material property','material name',#11459);
#5498=PROPERTY_DEFINITION('material property','density of part',#11459);
#5499=AXIS2_PLACEMENT_3D('',#7794,#6110,#6111);
#5500=AXIS2_PLACEMENT_3D('',#7795,#6112,#6113);
#5501=AXIS2_PLACEMENT_3D('',#7796,#6114,#6115);
#5502=AXIS2_PLACEMENT_3D('',#7805,#6120,#6121);
#5503=AXIS2_PLACEMENT_3D('',#7807,#6122,#6123);
#5504=AXIS2_PLACEMENT_3D('',#7810,#6125,#6126);
#5505=AXIS2_PLACEMENT_3D('',#7811,#6127,#6128);
#5506=AXIS2_PLACEMENT_3D('',#7817,#6132,#6133);
#5507=AXIS2_PLACEMENT_3D('',#7819,#6134,#6135);
#5508=AXIS2_PLACEMENT_3D('',#7822,#6137,#6138);
#5509=AXIS2_PLACEMENT_3D('',#7823,#6139,#6140);
#5510=AXIS2_PLACEMENT_3D('',#7829,#6144,#6145);
#5511=AXIS2_PLACEMENT_3D('',#7831,#6146,#6147);
#5512=AXIS2_PLACEMENT_3D('',#7834,#6149,#6150);
#5513=AXIS2_PLACEMENT_3D('',#7835,#6151,#6152);
#5514=AXIS2_PLACEMENT_3D('',#7841,#6156,#6157);
#5515=AXIS2_PLACEMENT_3D('',#7842,#6158,#6159);
#5516=AXIS2_PLACEMENT_3D('',#7843,#6160,#6161);
#5517=AXIS2_PLACEMENT_3D('',#7844,#6162,#6163);
#5518=AXIS2_PLACEMENT_3D('',#7853,#6168,#6169);
#5519=AXIS2_PLACEMENT_3D('',#7855,#6170,#6171);
#5520=AXIS2_PLACEMENT_3D('',#7858,#6173,#6174);
#5521=AXIS2_PLACEMENT_3D('',#7859,#6175,#6176);
#5522=AXIS2_PLACEMENT_3D('',#7865,#6180,#6181);
#5523=AXIS2_PLACEMENT_3D('',#7867,#6182,#6183);
#5524=AXIS2_PLACEMENT_3D('',#7870,#6185,#6186);
#5525=AXIS2_PLACEMENT_3D('',#7871,#6187,#6188);
#5526=AXIS2_PLACEMENT_3D('',#7877,#6192,#6193);
#5527=AXIS2_PLACEMENT_3D('',#7879,#6194,#6195);
#5528=AXIS2_PLACEMENT_3D('',#7882,#6197,#6198);
#5529=AXIS2_PLACEMENT_3D('',#7883,#6199,#6200);
#5530=AXIS2_PLACEMENT_3D('',#7889,#6204,#6205);
#5531=AXIS2_PLACEMENT_3D('',#7890,#6206,#6207);
#5532=AXIS2_PLACEMENT_3D('',#7891,#6208,#6209);
#5533=AXIS2_PLACEMENT_3D('',#7892,#6210,#6211);
#5534=AXIS2_PLACEMENT_3D('',#7901,#6216,#6217);
#5535=AXIS2_PLACEMENT_3D('',#7903,#6218,#6219);
#5536=AXIS2_PLACEMENT_3D('',#7906,#6221,#6222);
#5537=AXIS2_PLACEMENT_3D('',#7907,#6223,#6224);
#5538=AXIS2_PLACEMENT_3D('',#7913,#6228,#6229);
#5539=AXIS2_PLACEMENT_3D('',#7915,#6230,#6231);
#5540=AXIS2_PLACEMENT_3D('',#7918,#6233,#6234);
#5541=AXIS2_PLACEMENT_3D('',#7919,#6235,#6236);
#5542=AXIS2_PLACEMENT_3D('',#7925,#6240,#6241);
#5543=AXIS2_PLACEMENT_3D('',#7927,#6242,#6243);
#5544=AXIS2_PLACEMENT_3D('',#7930,#6245,#6246);
#5545=AXIS2_PLACEMENT_3D('',#7931,#6247,#6248);
#5546=AXIS2_PLACEMENT_3D('',#7937,#6252,#6253);
#5547=AXIS2_PLACEMENT_3D('',#7938,#6254,#6255);
#5548=AXIS2_PLACEMENT_3D('',#7939,#6256,#6257);
#5549=AXIS2_PLACEMENT_3D('',#7940,#6258,#6259);
#5550=AXIS2_PLACEMENT_3D('',#7949,#6264,#6265);
#5551=AXIS2_PLACEMENT_3D('',#7951,#6266,#6267);
#5552=AXIS2_PLACEMENT_3D('',#7954,#6269,#6270);
#5553=AXIS2_PLACEMENT_3D('',#7955,#6271,#6272);
#5554=AXIS2_PLACEMENT_3D('',#7961,#6276,#6277);
#5555=AXIS2_PLACEMENT_3D('',#7963,#6278,#6279);
#5556=AXIS2_PLACEMENT_3D('',#7966,#6281,#6282);
#5557=AXIS2_PLACEMENT_3D('',#7967,#6283,#6284);
#5558=AXIS2_PLACEMENT_3D('',#7973,#6288,#6289);
#5559=AXIS2_PLACEMENT_3D('',#7975,#6290,#6291);
#5560=AXIS2_PLACEMENT_3D('',#7978,#6293,#6294);
#5561=AXIS2_PLACEMENT_3D('',#7979,#6295,#6296);
#5562=AXIS2_PLACEMENT_3D('',#7985,#6300,#6301);
#5563=AXIS2_PLACEMENT_3D('',#7986,#6302,#6303);
#5564=AXIS2_PLACEMENT_3D('',#7987,#6304,#6305);
#5565=AXIS2_PLACEMENT_3D('',#7988,#6306,#6307);
#5566=AXIS2_PLACEMENT_3D('',#7990,#6308,#6309);
#5567=AXIS2_PLACEMENT_3D('',#7993,#6311,#6312);
#5568=AXIS2_PLACEMENT_3D('',#7994,#6313,#6314);
#5569=AXIS2_PLACEMENT_3D('',#7996,#6315,#6316);
#5570=AXIS2_PLACEMENT_3D('',#7999,#6318,#6319);
#5571=AXIS2_PLACEMENT_3D('',#8000,#6320,#6321);
#5572=AXIS2_PLACEMENT_3D('',#8014,#6322,#6323);
#5573=AXIS2_PLACEMENT_3D('',#8017,#6325,#6326);
#5574=AXIS2_PLACEMENT_3D('',#8018,#6327,#6328);
#5575=AXIS2_PLACEMENT_3D('',#8022,#6330,#6331);
#5576=AXIS2_PLACEMENT_3D('',#8023,#6332,#6333);
#5577=AXIS2_PLACEMENT_3D('',#8024,#6334,#6335);
#5578=AXIS2_PLACEMENT_3D('',#8030,#6339,#6340);
#5579=AXIS2_PLACEMENT_3D('',#8034,#6342,#6343);
#5580=AXIS2_PLACEMENT_3D('',#8035,#6344,#6345);
#5581=AXIS2_PLACEMENT_3D('',#8036,#6346,#6347);
#5582=AXIS2_PLACEMENT_3D('',#8042,#6351,#6352);
#5583=AXIS2_PLACEMENT_3D('',#8046,#6354,#6355);
#5584=AXIS2_PLACEMENT_3D('',#8047,#6356,#6357);
#5585=AXIS2_PLACEMENT_3D('',#8048,#6358,#6359);
#5586=AXIS2_PLACEMENT_3D('',#8054,#6363,#6364);
#5587=AXIS2_PLACEMENT_3D('',#8058,#6366,#6367);
#5588=AXIS2_PLACEMENT_3D('',#8059,#6368,#6369);
#5589=AXIS2_PLACEMENT_3D('',#8060,#6370,#6371);
#5590=AXIS2_PLACEMENT_3D('',#8066,#6375,#6376);
#5591=AXIS2_PLACEMENT_3D('',#8070,#6378,#6379);
#5592=AXIS2_PLACEMENT_3D('',#8071,#6380,#6381);
#5593=AXIS2_PLACEMENT_3D('',#8072,#6382,#6383);
#5594=AXIS2_PLACEMENT_3D('',#8078,#6387,#6388);
#5595=AXIS2_PLACEMENT_3D('',#8082,#6390,#6391);
#5596=AXIS2_PLACEMENT_3D('',#8083,#6392,#6393);
#5597=AXIS2_PLACEMENT_3D('',#8084,#6394,#6395);
#5598=AXIS2_PLACEMENT_3D('',#8090,#6399,#6400);
#5599=AXIS2_PLACEMENT_3D('',#8094,#6402,#6403);
#5600=AXIS2_PLACEMENT_3D('',#8095,#6404,#6405);
#5601=AXIS2_PLACEMENT_3D('',#8096,#6406,#6407);
#5602=AXIS2_PLACEMENT_3D('',#8102,#6411,#6412);
#5603=AXIS2_PLACEMENT_3D('',#8106,#6414,#6415);
#5604=AXIS2_PLACEMENT_3D('',#8107,#6416,#6417);
#5605=AXIS2_PLACEMENT_3D('',#8108,#6418,#6419);
#5606=AXIS2_PLACEMENT_3D('',#8114,#6423,#6424);
#5607=AXIS2_PLACEMENT_3D('',#8116,#6425,#6426);
#5608=AXIS2_PLACEMENT_3D('',#8119,#6428,#6429);
#5609=AXIS2_PLACEMENT_3D('',#8120,#6430,#6431);
#5610=AXIS2_PLACEMENT_3D('',#8126,#6435,#6436);
#5611=AXIS2_PLACEMENT_3D('',#8128,#6437,#6438);
#5612=AXIS2_PLACEMENT_3D('',#8131,#6440,#6441);
#5613=AXIS2_PLACEMENT_3D('',#8132,#6442,#6443);
#5614=AXIS2_PLACEMENT_3D('',#8138,#6447,#6448);
#5615=AXIS2_PLACEMENT_3D('',#8140,#6449,#6450);
#5616=AXIS2_PLACEMENT_3D('',#8143,#6452,#6453);
#5617=AXIS2_PLACEMENT_3D('',#8144,#6454,#6455);
#5618=AXIS2_PLACEMENT_3D('',#8150,#6459,#6460);
#5619=AXIS2_PLACEMENT_3D('',#8152,#6461,#6462);
#5620=AXIS2_PLACEMENT_3D('',#8155,#6464,#6465);
#5621=AXIS2_PLACEMENT_3D('',#8156,#6466,#6467);
#5622=AXIS2_PLACEMENT_3D('',#8162,#6471,#6472);
#5623=AXIS2_PLACEMENT_3D('',#8164,#6473,#6474);
#5624=AXIS2_PLACEMENT_3D('',#8167,#6476,#6477);
#5625=AXIS2_PLACEMENT_3D('',#8168,#6478,#6479);
#5626=AXIS2_PLACEMENT_3D('',#8174,#6483,#6484);
#5627=AXIS2_PLACEMENT_3D('',#8176,#6485,#6486);
#5628=AXIS2_PLACEMENT_3D('',#8179,#6488,#6489);
#5629=AXIS2_PLACEMENT_3D('',#8180,#6490,#6491);
#5630=AXIS2_PLACEMENT_3D('',#8186,#6495,#6496);
#5631=AXIS2_PLACEMENT_3D('',#8188,#6497,#6498);
#5632=AXIS2_PLACEMENT_3D('',#8191,#6500,#6501);
#5633=AXIS2_PLACEMENT_3D('',#8192,#6502,#6503);
#5634=AXIS2_PLACEMENT_3D('',#8198,#6507,#6508);
#5635=AXIS2_PLACEMENT_3D('',#8200,#6509,#6510);
#5636=AXIS2_PLACEMENT_3D('',#8203,#6512,#6513);
#5637=AXIS2_PLACEMENT_3D('',#8204,#6514,#6515);
#5638=AXIS2_PLACEMENT_3D('',#8210,#6519,#6520);
#5639=AXIS2_PLACEMENT_3D('',#8214,#6522,#6523);
#5640=AXIS2_PLACEMENT_3D('',#8215,#6524,#6525);
#5641=AXIS2_PLACEMENT_3D('',#8216,#6526,#6527);
#5642=AXIS2_PLACEMENT_3D('',#8217,#6528,#6529);
#5643=AXIS2_PLACEMENT_3D('',#8218,#6530,#6531);
#5644=AXIS2_PLACEMENT_3D('',#8219,#6532,#6533);
#5645=AXIS2_PLACEMENT_3D('',#8225,#6537,#6538);
#5646=AXIS2_PLACEMENT_3D('',#8228,#6540,#6541);
#5647=AXIS2_PLACEMENT_3D('',#8229,#6542,#6543);
#5648=AXIS2_PLACEMENT_3D('',#8233,#6546,#6547);
#5649=AXIS2_PLACEMENT_3D('',#8236,#6549,#6550);
#5650=AXIS2_PLACEMENT_3D('',#8237,#6551,#6552);
#5651=AXIS2_PLACEMENT_3D('',#8241,#6555,#6556);
#5652=AXIS2_PLACEMENT_3D('',#8244,#6558,#6559);
#5653=AXIS2_PLACEMENT_3D('',#8245,#6560,#6561);
#5654=AXIS2_PLACEMENT_3D('',#8249,#6564,#6565);
#5655=AXIS2_PLACEMENT_3D('',#8252,#6567,#6568);
#5656=AXIS2_PLACEMENT_3D('',#8253,#6569,#6570);
#5657=AXIS2_PLACEMENT_3D('',#8257,#6573,#6574);
#5658=AXIS2_PLACEMENT_3D('',#8260,#6576,#6577);
#5659=AXIS2_PLACEMENT_3D('',#8261,#6578,#6579);
#5660=AXIS2_PLACEMENT_3D('',#8265,#6582,#6583);
#5661=AXIS2_PLACEMENT_3D('',#8268,#6585,#6586);
#5662=AXIS2_PLACEMENT_3D('',#8269,#6587,#6588);
#5663=AXIS2_PLACEMENT_3D('',#8273,#6591,#6592);
#5664=AXIS2_PLACEMENT_3D('',#8276,#6594,#6595);
#5665=AXIS2_PLACEMENT_3D('',#8277,#6596,#6597);
#5666=AXIS2_PLACEMENT_3D('',#8281,#6600,#6601);
#5667=AXIS2_PLACEMENT_3D('',#8284,#6603,#6604);
#5668=AXIS2_PLACEMENT_3D('',#8285,#6605,#6606);
#5669=AXIS2_PLACEMENT_3D('',#8288,#6608,#6609);
#5670=AXIS2_PLACEMENT_3D('',#8289,#6610,#6611);
#5671=AXIS2_PLACEMENT_3D('',#8292,#6613,#6614);
#5672=AXIS2_PLACEMENT_3D('',#8293,#6615,#6616);
#5673=AXIS2_PLACEMENT_3D('',#8295,#6617,#6618);
#5674=AXIS2_PLACEMENT_3D('',#8297,#6619,#6620);
#5675=AXIS2_PLACEMENT_3D('',#8299,#6621,#6622);
#5676=AXIS2_PLACEMENT_3D('',#8301,#6623,#6624);
#5677=AXIS2_PLACEMENT_3D('',#8303,#6625,#6626);
#5678=AXIS2_PLACEMENT_3D('',#8304,#6627,#6628);
#5679=AXIS2_PLACEMENT_3D('',#8317,#6629,#6630);
#5680=AXIS2_PLACEMENT_3D('',#8319,#6632,#6633);
#5681=AXIS2_PLACEMENT_3D('',#8322,#6635,#6636);
#5682=AXIS2_PLACEMENT_3D('',#8323,#6637,#6638);
#5683=AXIS2_PLACEMENT_3D('',#8327,#6641,#6642);
#5684=AXIS2_PLACEMENT_3D('',#8330,#6644,#6645);
#5685=AXIS2_PLACEMENT_3D('',#8331,#6646,#6647);
#5686=AXIS2_PLACEMENT_3D('',#8335,#6650,#6651);
#5687=AXIS2_PLACEMENT_3D('',#8338,#6653,#6654);
#5688=AXIS2_PLACEMENT_3D('',#8339,#6655,#6656);
#5689=AXIS2_PLACEMENT_3D('',#8343,#6659,#6660);
#5690=AXIS2_PLACEMENT_3D('',#8346,#6662,#6663);
#5691=AXIS2_PLACEMENT_3D('',#8347,#6664,#6665);
#5692=AXIS2_PLACEMENT_3D('',#8351,#6668,#6669);
#5693=AXIS2_PLACEMENT_3D('',#8354,#6671,#6672);
#5694=AXIS2_PLACEMENT_3D('',#8355,#6673,#6674);
#5695=AXIS2_PLACEMENT_3D('',#8359,#6677,#6678);
#5696=AXIS2_PLACEMENT_3D('',#8362,#6680,#6681);
#5697=AXIS2_PLACEMENT_3D('',#8363,#6682,#6683);
#5698=AXIS2_PLACEMENT_3D('',#8367,#6686,#6687);
#5699=AXIS2_PLACEMENT_3D('',#8370,#6689,#6690);
#5700=AXIS2_PLACEMENT_3D('',#8371,#6691,#6692);
#5701=AXIS2_PLACEMENT_3D('',#8375,#6695,#6696);
#5702=AXIS2_PLACEMENT_3D('',#8378,#6698,#6699);
#5703=AXIS2_PLACEMENT_3D('',#8379,#6700,#6701);
#5704=AXIS2_PLACEMENT_3D('',#8383,#6704,#6705);
#5705=AXIS2_PLACEMENT_3D('',#8387,#6707,#6708);
#5706=AXIS2_PLACEMENT_3D('',#8388,#6709,#6710);
#5707=AXIS2_PLACEMENT_3D('',#8389,#6711,#6712);
#5708=AXIS2_PLACEMENT_3D('',#8395,#6716,#6717);
#5709=AXIS2_PLACEMENT_3D('',#8397,#6718,#6719);
#5710=AXIS2_PLACEMENT_3D('',#8400,#6721,#6722);
#5711=AXIS2_PLACEMENT_3D('',#8401,#6723,#6724);
#5712=AXIS2_PLACEMENT_3D('',#8407,#6728,#6729);
#5713=AXIS2_PLACEMENT_3D('',#8409,#6730,#6731);
#5714=AXIS2_PLACEMENT_3D('',#8412,#6733,#6734);
#5715=AXIS2_PLACEMENT_3D('',#8413,#6735,#6736);
#5716=AXIS2_PLACEMENT_3D('',#8419,#6740,#6741);
#5717=AXIS2_PLACEMENT_3D('',#8421,#6742,#6743);
#5718=AXIS2_PLACEMENT_3D('',#8424,#6745,#6746);
#5719=AXIS2_PLACEMENT_3D('',#8425,#6747,#6748);
#5720=AXIS2_PLACEMENT_3D('',#8431,#6752,#6753);
#5721=AXIS2_PLACEMENT_3D('',#8433,#6754,#6755);
#5722=AXIS2_PLACEMENT_3D('',#8436,#6757,#6758);
#5723=AXIS2_PLACEMENT_3D('',#8437,#6759,#6760);
#5724=AXIS2_PLACEMENT_3D('',#8443,#6764,#6765);
#5725=AXIS2_PLACEMENT_3D('',#8445,#6766,#6767);
#5726=AXIS2_PLACEMENT_3D('',#8448,#6769,#6770);
#5727=AXIS2_PLACEMENT_3D('',#8449,#6771,#6772);
#5728=AXIS2_PLACEMENT_3D('',#8455,#6776,#6777);
#5729=AXIS2_PLACEMENT_3D('',#8457,#6778,#6779);
#5730=AXIS2_PLACEMENT_3D('',#8460,#6781,#6782);
#5731=AXIS2_PLACEMENT_3D('',#8461,#6783,#6784);
#5732=AXIS2_PLACEMENT_3D('',#8467,#6788,#6789);
#5733=AXIS2_PLACEMENT_3D('',#8469,#6790,#6791);
#5734=AXIS2_PLACEMENT_3D('',#8472,#6793,#6794);
#5735=AXIS2_PLACEMENT_3D('',#8473,#6795,#6796);
#5736=AXIS2_PLACEMENT_3D('',#8479,#6800,#6801);
#5737=AXIS2_PLACEMENT_3D('',#8482,#6803,#6804);
#5738=AXIS2_PLACEMENT_3D('',#8483,#6805,#6806);
#5739=AXIS2_PLACEMENT_3D('',#8484,#6807,#6808);
#5740=AXIS2_PLACEMENT_3D('',#8485,#6809,#6810);
#5741=AXIS2_PLACEMENT_3D('',#8486,#6811,#6812);
#5742=AXIS2_PLACEMENT_3D('',#8489,#6815,#6816);
#5743=AXIS2_PLACEMENT_3D('',#8491,#6818,#6819);
#5744=AXIS2_PLACEMENT_3D('',#8493,#6821,#6822);
#5745=AXIS2_PLACEMENT_3D('',#8495,#6824,#6825);
#5746=AXIS2_PLACEMENT_3D('',#8497,#6827,#6828);
#5747=AXIS2_PLACEMENT_3D('',#8499,#6830,#6831);
#5748=AXIS2_PLACEMENT_3D('',#8501,#6833,#6834);
#5749=AXIS2_PLACEMENT_3D('',#8503,#6836,#6837);
#5750=AXIS2_PLACEMENT_3D('',#8505,#6839,#6840);
#5751=AXIS2_PLACEMENT_3D('',#8507,#6842,#6843);
#5752=AXIS2_PLACEMENT_3D('',#8509,#6845,#6846);
#5753=AXIS2_PLACEMENT_3D('',#8511,#6848,#6849);
#5754=AXIS2_PLACEMENT_3D('',#8513,#6851,#6852);
#5755=AXIS2_PLACEMENT_3D('',#8515,#6854,#6855);
#5756=AXIS2_PLACEMENT_3D('',#8517,#6857,#6858);
#5757=AXIS2_PLACEMENT_3D('',#8518,#6859,#6860);
#5758=AXIS2_PLACEMENT_3D('',#8520,#6861,#6862);
#5759=AXIS2_PLACEMENT_3D('',#8522,#6863,#6864);
#5760=AXIS2_PLACEMENT_3D('',#8524,#6865,#6866);
#5761=AXIS2_PLACEMENT_3D('',#8525,#6867,#6868);
#5762=AXIS2_PLACEMENT_3D('',#8527,#6869,#6870);
#5763=AXIS2_PLACEMENT_3D('',#8528,#6871,#6872);
#5764=AXIS2_PLACEMENT_3D('',#8529,#6873,#6874);
#5765=AXIS2_PLACEMENT_3D('',#8530,#6875,#6876);
#5766=AXIS2_PLACEMENT_3D('',#8532,#6877,#6878);
#5767=AXIS2_PLACEMENT_3D('',#8533,#6879,#6880);
#5768=AXIS2_PLACEMENT_3D('',#8535,#6881,#6882);
#5769=AXIS2_PLACEMENT_3D('',#8537,#6884,#6885);
#5770=AXIS2_PLACEMENT_3D('',#8539,#6887,#6888);
#5771=AXIS2_PLACEMENT_3D('',#8541,#6889,#6890);
#5772=AXIS2_PLACEMENT_3D('',#8543,#6892,#6893);
#5773=AXIS2_PLACEMENT_3D('',#8545,#6895,#6896);
#5774=AXIS2_PLACEMENT_3D('',#8548,#6898,#6899);
#5775=AXIS2_PLACEMENT_3D('',#8549,#6900,#6901);
#5776=AXIS2_PLACEMENT_3D('',#8551,#6903,#6904);
#5777=AXIS2_PLACEMENT_3D('',#8553,#6906,#6907);
#5778=AXIS2_PLACEMENT_3D('',#8555,#6909,#6910);
#5779=AXIS2_PLACEMENT_3D('',#8556,#6911,#6912);
#5780=AXIS2_PLACEMENT_3D('',#8557,#6913,#6914);
#5781=AXIS2_PLACEMENT_3D('',#8559,#6915,#6916);
#5782=AXIS2_PLACEMENT_3D('',#8562,#6918,#6919);
#5783=AXIS2_PLACEMENT_3D('',#8563,#6920,#6921);
#5784=AXIS2_PLACEMENT_3D('',#8566,#6923,#6924);
#5785=AXIS2_PLACEMENT_3D('',#8567,#6925,#6926);
#5786=AXIS2_PLACEMENT_3D('',#8568,#6927,#6928);
#5787=AXIS2_PLACEMENT_3D('',#8571,#6930,#6931);
#5788=AXIS2_PLACEMENT_3D('',#8572,#6932,#6933);
#5789=AXIS2_PLACEMENT_3D('',#8573,#6934,#6935);
#5790=AXIS2_PLACEMENT_3D('',#8574,#6936,#6937);
#5791=AXIS2_PLACEMENT_3D('',#8576,#6938,#6939);
#5792=AXIS2_PLACEMENT_3D('',#8577,#6940,#6941);
#5793=AXIS2_PLACEMENT_3D('',#8580,#6942,#6943);
#5794=AXIS2_PLACEMENT_3D('',#9107,#6944,#6945);
#5795=AXIS2_PLACEMENT_3D('',#9108,#6946,#6947);
#5796=AXIS2_PLACEMENT_3D('',#9109,#6948,#6949);
#5797=AXIS2_PLACEMENT_3D('',#9110,#6950,#6951);
#5798=AXIS2_PLACEMENT_3D('',#9112,#6952,#6953);
#5799=AXIS2_PLACEMENT_3D('',#9114,#6954,#6955);
#5800=AXIS2_PLACEMENT_3D('',#9115,#6956,#6957);
#5801=AXIS2_PLACEMENT_3D('',#9117,#6958,#6959);
#5802=AXIS2_PLACEMENT_3D('',#9119,#6960,#6961);
#5803=AXIS2_PLACEMENT_3D('',#9120,#6962,#6963);
#5804=AXIS2_PLACEMENT_3D('',#9121,#6964,#6965);
#5805=AXIS2_PLACEMENT_3D('',#9124,#6967,#6968);
#5806=AXIS2_PLACEMENT_3D('',#9125,#6969,#6970);
#5807=AXIS2_PLACEMENT_3D('',#9126,#6971,#6972);
#5808=AXIS2_PLACEMENT_3D('',#9135,#6977,#6978);
#5809=AXIS2_PLACEMENT_3D('',#9141,#6982,#6983);
#5810=AXIS2_PLACEMENT_3D('',#9147,#6987,#6988);
#5811=AXIS2_PLACEMENT_3D('',#9153,#6992,#6993);
#5812=AXIS2_PLACEMENT_3D('',#9159,#6997,#6998);
#5813=AXIS2_PLACEMENT_3D('',#9162,#7001,#7002);
#5814=AXIS2_PLACEMENT_3D('',#9163,#7003,#7004);
#5815=AXIS2_PLACEMENT_3D('',#9165,#7005,#7006);
#5816=AXIS2_PLACEMENT_3D('',#9167,#7008,#7009);
#5817=AXIS2_PLACEMENT_3D('',#9168,#7010,#7011);
#5818=AXIS2_PLACEMENT_3D('',#9169,#7012,#7013);
#5819=AXIS2_PLACEMENT_3D('',#9171,#7014,#7015);
#5820=AXIS2_PLACEMENT_3D('',#9173,#7016,#7017);
#5821=AXIS2_PLACEMENT_3D('',#9174,#7018,#7019);
#5822=AXIS2_PLACEMENT_3D('',#9179,#7021,#7022);
#5823=AXIS2_PLACEMENT_3D('',#9183,#7024,#7025);
#5824=AXIS2_PLACEMENT_3D('',#9187,#7027,#7028);
#5825=AXIS2_PLACEMENT_3D('',#9191,#7030,#7031);
#5826=AXIS2_PLACEMENT_3D('',#9195,#7033,#7034);
#5827=AXIS2_PLACEMENT_3D('',#9199,#7036,#7037);
#5828=AXIS2_PLACEMENT_3D('',#9203,#7039,#7040);
#5829=AXIS2_PLACEMENT_3D('',#9205,#7041,#7042);
#5830=AXIS2_PLACEMENT_3D('',#9209,#7044,#7045);
#5831=AXIS2_PLACEMENT_3D('',#9213,#7047,#7048);
#5832=AXIS2_PLACEMENT_3D('',#9217,#7050,#7051);
#5833=AXIS2_PLACEMENT_3D('',#9219,#7052,#7053);
#5834=AXIS2_PLACEMENT_3D('',#9223,#7055,#7056);
#5835=AXIS2_PLACEMENT_3D('',#9227,#7058,#7059);
#5836=AXIS2_PLACEMENT_3D('',#9230,#7061,#7062);
#5837=AXIS2_PLACEMENT_3D('',#9232,#7063,#7064);
#5838=AXIS2_PLACEMENT_3D('',#9234,#7065,#7066);
#5839=AXIS2_PLACEMENT_3D('',#9236,#7067,#7068);
#5840=AXIS2_PLACEMENT_3D('',#9238,#7069,#7070);
#5841=AXIS2_PLACEMENT_3D('',#9240,#7071,#7072);
#5842=AXIS2_PLACEMENT_3D('',#9242,#7073,#7074);
#5843=AXIS2_PLACEMENT_3D('',#9244,#7075,#7076);
#5844=AXIS2_PLACEMENT_3D('',#9245,#7077,#7078);
#5845=AXIS2_PLACEMENT_3D('',#9247,#7079,#7080);
#5846=AXIS2_PLACEMENT_3D('',#9248,#7081,#7082);
#5847=AXIS2_PLACEMENT_3D('',#9250,#7083,#7084);
#5848=AXIS2_PLACEMENT_3D('',#9251,#7085,#7086);
#5849=AXIS2_PLACEMENT_3D('',#9254,#7088,#7089);
#5850=AXIS2_PLACEMENT_3D('',#9255,#7090,#7091);
#5851=AXIS2_PLACEMENT_3D('',#9257,#7092,#7093);
#5852=AXIS2_PLACEMENT_3D('',#9259,#7095,#7096);
#5853=AXIS2_PLACEMENT_3D('',#9262,#7098,#7099);
#5854=AXIS2_PLACEMENT_3D('',#9263,#7100,#7101);
#5855=AXIS2_PLACEMENT_3D('',#9265,#7102,#7103);
#5856=AXIS2_PLACEMENT_3D('',#9267,#7105,#7106);
#5857=AXIS2_PLACEMENT_3D('',#9269,#7107,#7108);
#5858=AXIS2_PLACEMENT_3D('',#9271,#7110,#7111);
#5859=AXIS2_PLACEMENT_3D('',#9273,#7112,#7113);
#5860=AXIS2_PLACEMENT_3D('',#9275,#7115,#7116);
#5861=AXIS2_PLACEMENT_3D('',#9277,#7117,#7118);
#5862=AXIS2_PLACEMENT_3D('',#9279,#7120,#7121);
#5863=AXIS2_PLACEMENT_3D('',#9281,#7122,#7123);
#5864=AXIS2_PLACEMENT_3D('',#9283,#7125,#7126);
#5865=AXIS2_PLACEMENT_3D('',#9286,#7128,#7129);
#5866=AXIS2_PLACEMENT_3D('',#9287,#7130,#7131);
#5867=AXIS2_PLACEMENT_3D('',#9292,#7133,#7134);
#5868=AXIS2_PLACEMENT_3D('',#9296,#7136,#7137);
#5869=AXIS2_PLACEMENT_3D('',#9300,#7139,#7140);
#5870=AXIS2_PLACEMENT_3D('',#9304,#7142,#7143);
#5871=AXIS2_PLACEMENT_3D('',#9306,#7144,#7145);
#5872=AXIS2_PLACEMENT_3D('',#9310,#7147,#7148);
#5873=AXIS2_PLACEMENT_3D('',#9314,#7150,#7151);
#5874=AXIS2_PLACEMENT_3D('',#9318,#7153,#7154);
#5875=AXIS2_PLACEMENT_3D('',#9320,#7155,#7156);
#5876=AXIS2_PLACEMENT_3D('',#9324,#7158,#7159);
#5877=AXIS2_PLACEMENT_3D('',#9328,#7161,#7162);
#5878=AXIS2_PLACEMENT_3D('',#9332,#7164,#7165);
#5879=AXIS2_PLACEMENT_3D('',#9336,#7167,#7168);
#5880=AXIS2_PLACEMENT_3D('',#9340,#7170,#7171);
#5881=AXIS2_PLACEMENT_3D('',#9343,#7173,#7174);
#5882=AXIS2_PLACEMENT_3D('',#9345,#7175,#7176);
#5883=AXIS2_PLACEMENT_3D('',#9347,#7177,#7178);
#5884=AXIS2_PLACEMENT_3D('',#9349,#7179,#7180);
#5885=AXIS2_PLACEMENT_3D('',#9351,#7181,#7182);
#5886=AXIS2_PLACEMENT_3D('',#9352,#7183,#7184);
#5887=AXIS2_PLACEMENT_3D('',#9354,#7186,#7187);
#5888=AXIS2_PLACEMENT_3D('',#9356,#7189,#7190);
#5889=AXIS2_PLACEMENT_3D('',#9358,#7192,#7193);
#5890=AXIS2_PLACEMENT_3D('',#9364,#7197,#7198);
#5891=AXIS2_PLACEMENT_3D('',#9366,#7199,#7200);
#5892=AXIS2_PLACEMENT_3D('',#9368,#7202,#7203);
#5893=AXIS2_PLACEMENT_3D('',#9372,#7206,#7207);
#5894=AXIS2_PLACEMENT_3D('',#9374,#7208,#7209);
#5895=AXIS2_PLACEMENT_3D('',#9376,#7211,#7212);
#5896=AXIS2_PLACEMENT_3D('',#9380,#7215,#7216);
#5897=AXIS2_PLACEMENT_3D('',#9382,#7217,#7218);
#5898=AXIS2_PLACEMENT_3D('',#9384,#7220,#7221);
#5899=AXIS2_PLACEMENT_3D('',#9388,#7224,#7225);
#5900=AXIS2_PLACEMENT_3D('',#9391,#7227,#7228);
#5901=AXIS2_PLACEMENT_3D('',#9392,#7229,#7230);
#5902=AXIS2_PLACEMENT_3D('',#9394,#7231,#7232);
#5903=AXIS2_PLACEMENT_3D('',#9396,#7234,#7235);
#5904=AXIS2_PLACEMENT_3D('',#9400,#7238,#7239);
#5905=AXIS2_PLACEMENT_3D('',#9402,#7240,#7241);
#5906=AXIS2_PLACEMENT_3D('',#9404,#7243,#7244);
#5907=AXIS2_PLACEMENT_3D('',#9408,#7247,#7248);
#5908=AXIS2_PLACEMENT_3D('',#9410,#7249,#7250);
#5909=AXIS2_PLACEMENT_3D('',#9412,#7252,#7253);
#5910=AXIS2_PLACEMENT_3D('',#9416,#7256,#7257);
#5911=AXIS2_PLACEMENT_3D('',#9418,#7258,#7259);
#5912=AXIS2_PLACEMENT_3D('',#9420,#7261,#7262);
#5913=AXIS2_PLACEMENT_3D('',#9422,#7263,#7264);
#5914=AXIS2_PLACEMENT_3D('',#9424,#7266,#7267);
#5915=AXIS2_PLACEMENT_3D('',#9428,#7270,#7271);
#5916=AXIS2_PLACEMENT_3D('',#9430,#7272,#7273);
#5917=AXIS2_PLACEMENT_3D('',#9432,#7275,#7276);
#5918=AXIS2_PLACEMENT_3D('',#9436,#7279,#7280);
#5919=AXIS2_PLACEMENT_3D('',#9438,#7281,#7282);
#5920=AXIS2_PLACEMENT_3D('',#9440,#7284,#7285);
#5921=AXIS2_PLACEMENT_3D('',#9444,#7288,#7289);
#5922=AXIS2_PLACEMENT_3D('',#9446,#7290,#7291);
#5923=AXIS2_PLACEMENT_3D('',#9448,#7293,#7294);
#5924=AXIS2_PLACEMENT_3D('',#9452,#7297,#7298);
#5925=AXIS2_PLACEMENT_3D('',#9454,#7299,#7300);
#5926=AXIS2_PLACEMENT_3D('',#9456,#7302,#7303);
#5927=AXIS2_PLACEMENT_3D('',#9460,#7306,#7307);
#5928=AXIS2_PLACEMENT_3D('',#9462,#7308,#7309);
#5929=AXIS2_PLACEMENT_3D('',#9464,#7311,#7312);
#5930=AXIS2_PLACEMENT_3D('',#9468,#7315,#7316);
#5931=AXIS2_PLACEMENT_3D('',#9469,#7317,#7318);
#5932=AXIS2_PLACEMENT_3D('',#9470,#7319,#7320);
#5933=AXIS2_PLACEMENT_3D('',#9476,#7324,#7325);
#5934=AXIS2_PLACEMENT_3D('',#9479,#7327,#7328);
#5935=AXIS2_PLACEMENT_3D('',#9480,#7329,#7330);
#5936=AXIS2_PLACEMENT_3D('',#9484,#7333,#7334);
#5937=AXIS2_PLACEMENT_3D('',#9487,#7336,#7337);
#5938=AXIS2_PLACEMENT_3D('',#9488,#7338,#7339);
#5939=AXIS2_PLACEMENT_3D('',#9492,#7342,#7343);
#5940=AXIS2_PLACEMENT_3D('',#9495,#7345,#7346);
#5941=AXIS2_PLACEMENT_3D('',#9496,#7347,#7348);
#5942=AXIS2_PLACEMENT_3D('',#9499,#7350,#7351);
#5943=AXIS2_PLACEMENT_3D('',#9500,#7352,#7353);
#5944=AXIS2_PLACEMENT_3D('',#9504,#7356,#7357);
#5945=AXIS2_PLACEMENT_3D('',#9507,#7359,#7360);
#5946=AXIS2_PLACEMENT_3D('',#9508,#7361,#7362);
#5947=AXIS2_PLACEMENT_3D('',#9512,#7365,#7366);
#5948=AXIS2_PLACEMENT_3D('',#9515,#7368,#7369);
#5949=AXIS2_PLACEMENT_3D('',#9516,#7370,#7371);
#5950=AXIS2_PLACEMENT_3D('',#9520,#7374,#7375);
#5951=AXIS2_PLACEMENT_3D('',#9523,#7377,#7378);
#5952=AXIS2_PLACEMENT_3D('',#9524,#7379,#7380);
#5953=AXIS2_PLACEMENT_3D('',#9528,#7383,#7384);
#5954=AXIS2_PLACEMENT_3D('',#9531,#7387,#7388);
#5955=AXIS2_PLACEMENT_3D('',#9533,#7390,#7391);
#5956=AXIS2_PLACEMENT_3D('',#9535,#7393,#7394);
#5957=AXIS2_PLACEMENT_3D('',#9537,#7396,#7397);
#5958=AXIS2_PLACEMENT_3D('',#9539,#7399,#7400);
#5959=AXIS2_PLACEMENT_3D('',#9541,#7402,#7403);
#5960=AXIS2_PLACEMENT_3D('',#9543,#7405,#7406);
#5961=AXIS2_PLACEMENT_3D('',#9545,#7408,#7409);
#5962=AXIS2_PLACEMENT_3D('',#9547,#7411,#7412);
#5963=AXIS2_PLACEMENT_3D('',#9549,#7414,#7415);
#5964=AXIS2_PLACEMENT_3D('',#9551,#7417,#7418);
#5965=AXIS2_PLACEMENT_3D('',#9553,#7420,#7421);
#5966=AXIS2_PLACEMENT_3D('',#9555,#7423,#7424);
#5967=AXIS2_PLACEMENT_3D('',#9557,#7426,#7427);
#5968=AXIS2_PLACEMENT_3D('',#9560,#7429,#7430);
#5969=AXIS2_PLACEMENT_3D('',#9561,#7431,#7432);
#5970=AXIS2_PLACEMENT_3D('',#9564,#7434,#7435);
#5971=AXIS2_PLACEMENT_3D('',#9565,#7436,#7437);
#5972=AXIS2_PLACEMENT_3D('',#9569,#7440,#7441);
#5973=AXIS2_PLACEMENT_3D('',#9572,#7443,#7444);
#5974=AXIS2_PLACEMENT_3D('',#9573,#7445,#7446);
#5975=AXIS2_PLACEMENT_3D('',#9577,#7449,#7450);
#5976=AXIS2_PLACEMENT_3D('',#9580,#7452,#7453);
#5977=AXIS2_PLACEMENT_3D('',#9581,#7454,#7455);
#5978=AXIS2_PLACEMENT_3D('',#9585,#7458,#7459);
#5979=AXIS2_PLACEMENT_3D('',#9588,#7461,#7462);
#5980=AXIS2_PLACEMENT_3D('',#9589,#7463,#7464);
#5981=AXIS2_PLACEMENT_3D('',#9593,#7467,#7468);
#5982=AXIS2_PLACEMENT_3D('',#9596,#7470,#7471);
#5983=AXIS2_PLACEMENT_3D('',#9597,#7472,#7473);
#5984=AXIS2_PLACEMENT_3D('',#9601,#7476,#7477);
#5985=AXIS2_PLACEMENT_3D('',#9604,#7479,#7480);
#5986=AXIS2_PLACEMENT_3D('',#9605,#7481,#7482);
#5987=AXIS2_PLACEMENT_3D('',#9609,#7485,#7486);
#5988=AXIS2_PLACEMENT_3D('',#9610,#7487,#7488);
#5989=AXIS2_PLACEMENT_3D('',#9611,#7489,#7490);
#5990=AXIS2_PLACEMENT_3D('',#9614,#7493,#7494);
#5991=AXIS2_PLACEMENT_3D('',#9616,#7496,#7497);
#5992=AXIS2_PLACEMENT_3D('',#9618,#7499,#7500);
#5993=AXIS2_PLACEMENT_3D('',#9620,#7502,#7503);
#5994=AXIS2_PLACEMENT_3D('',#9622,#7505,#7506);
#5995=AXIS2_PLACEMENT_3D('',#9624,#7508,#7509);
#5996=AXIS2_PLACEMENT_3D('',#9626,#7511,#7512);
#5997=AXIS2_PLACEMENT_3D('',#9628,#7514,#7515);
#5998=AXIS2_PLACEMENT_3D('',#9630,#7517,#7518);
#5999=AXIS2_PLACEMENT_3D('',#9632,#7520,#7521);
#6000=AXIS2_PLACEMENT_3D('',#9634,#7523,#7524);
#6001=AXIS2_PLACEMENT_3D('',#9636,#7526,#7527);
#6002=AXIS2_PLACEMENT_3D('',#9637,#7528,#7529);
#6003=AXIS2_PLACEMENT_3D('',#9638,#7530,#7531);
#6004=AXIS2_PLACEMENT_3D('',#9640,#7533,#7534);
#6005=AXIS2_PLACEMENT_3D('',#9641,#7535,#7536);
#6006=AXIS2_PLACEMENT_3D('',#9643,#7537,#7538);
#6007=AXIS2_PLACEMENT_3D('',#9646,#7540,#7541);
#6008=AXIS2_PLACEMENT_3D('',#9647,#7542,#7543);
#6009=AXIS2_PLACEMENT_3D('',#9650,#7545,#7546);
#6010=AXIS2_PLACEMENT_3D('',#9651,#7547,#7548);
#6011=AXIS2_PLACEMENT_3D('',#9652,#7549,#7550);
#6012=AXIS2_PLACEMENT_3D('',#9655,#7552,#7553);
#6013=AXIS2_PLACEMENT_3D('',#9656,#7554,#7555);
#6014=AXIS2_PLACEMENT_3D('',#9657,#7556,#7557);
#6015=AXIS2_PLACEMENT_3D('',#9658,#7558,#7559);
#6016=AXIS2_PLACEMENT_3D('',#9660,#7560,#7561);
#6017=AXIS2_PLACEMENT_3D('',#9662,#7562,#7563);
#6018=AXIS2_PLACEMENT_3D('',#9663,#7564,#7565);
#6019=AXIS2_PLACEMENT_3D('',#9665,#7566,#7567);
#6020=AXIS2_PLACEMENT_3D('',#9667,#7568,#7569);
#6021=AXIS2_PLACEMENT_3D('',#9668,#7570,#7571);
#6022=AXIS2_PLACEMENT_3D('',#9669,#7572,#7573);
#6023=AXIS2_PLACEMENT_3D('',#9672,#7575,#7576);
#6024=AXIS2_PLACEMENT_3D('',#9673,#7577,#7578);
#6025=AXIS2_PLACEMENT_3D('',#9674,#7579,#7580);
#6026=AXIS2_PLACEMENT_3D('',#9683,#7585,#7586);
#6027=AXIS2_PLACEMENT_3D('',#9689,#7590,#7591);
#6028=AXIS2_PLACEMENT_3D('',#9695,#7595,#7596);
#6029=AXIS2_PLACEMENT_3D('',#9701,#7600,#7601);
#6030=AXIS2_PLACEMENT_3D('',#9707,#7605,#7606);
#6031=AXIS2_PLACEMENT_3D('',#9710,#7609,#7610);
#6032=AXIS2_PLACEMENT_3D('',#9711,#7611,#7612);
#6033=AXIS2_PLACEMENT_3D('',#9713,#7613,#7614);
#6034=AXIS2_PLACEMENT_3D('',#9715,#7616,#7617);
#6035=AXIS2_PLACEMENT_3D('',#9716,#7618,#7619);
#6036=AXIS2_PLACEMENT_3D('',#9717,#7620,#7621);
#6037=AXIS2_PLACEMENT_3D('',#9719,#7622,#7623);
#6038=AXIS2_PLACEMENT_3D('',#9720,#7624,#7625);
#6039=AXIS2_PLACEMENT_3D('',#9723,#7626,#7627);
#6040=AXIS2_PLACEMENT_3D('',#10250,#7628,#7629);
#6041=AXIS2_PLACEMENT_3D('',#10251,#7630,#7631);
#6042=AXIS2_PLACEMENT_3D('',#10252,#7632,#7633);
#6043=AXIS2_PLACEMENT_3D('',#10253,#7634,#7635);
#6044=AXIS2_PLACEMENT_3D('',#10255,#7636,#7637);
#6045=AXIS2_PLACEMENT_3D('',#10256,#7638,#7639);
#6046=AXIS2_PLACEMENT_3D('',#10259,#7640,#7641);
#6047=AXIS2_PLACEMENT_3D('',#10786,#7642,#7643);
#6048=AXIS2_PLACEMENT_3D('',#10787,#7644,#7645);
#6049=AXIS2_PLACEMENT_3D('',#10788,#7646,#7647);
#6050=AXIS2_PLACEMENT_3D('',#10789,#7648,#7649);
#6051=AXIS2_PLACEMENT_3D('',#10791,#7650,#7651);
#6052=AXIS2_PLACEMENT_3D('',#10794,#7653,#7654);
#6053=AXIS2_PLACEMENT_3D('',#10795,#7655,#7656);
#6054=AXIS2_PLACEMENT_3D('',#10798,#7658,#7659);
#6055=AXIS2_PLACEMENT_3D('',#10799,#7660,#7661);
#6056=AXIS2_PLACEMENT_3D('',#10800,#7662,#7663);
#6057=AXIS2_PLACEMENT_3D('',#10803,#7665,#7666);
#6058=AXIS2_PLACEMENT_3D('',#10804,#7667,#7668);
#6059=AXIS2_PLACEMENT_3D('',#10805,#7669,#7670);
#6060=AXIS2_PLACEMENT_3D('',#10806,#7671,#7672);
#6061=AXIS2_PLACEMENT_3D('',#10808,#7673,#7674);
#6062=AXIS2_PLACEMENT_3D('',#10809,#7675,#7676);
#6063=AXIS2_PLACEMENT_3D('',#10812,#7677,#7678);
#6064=AXIS2_PLACEMENT_3D('',#11265,#7679,#7680);
#6065=AXIS2_PLACEMENT_3D('',#11266,#7681,#7682);
#6066=AXIS2_PLACEMENT_3D('',#11267,#7683,#7684);
#6067=AXIS2_PLACEMENT_3D('',#11268,#7685,#7686);
#6068=AXIS2_PLACEMENT_3D('',#11270,#7687,#7688);
#6069=AXIS2_PLACEMENT_3D('',#11273,#7690,#7691);
#6070=AXIS2_PLACEMENT_3D('',#11274,#7692,#7693);
#6071=AXIS2_PLACEMENT_3D('',#11277,#7695,#7696);
#6072=AXIS2_PLACEMENT_3D('',#11278,#7697,#7698);
#6073=AXIS2_PLACEMENT_3D('',#11279,#7699,#7700);
#6074=AXIS2_PLACEMENT_3D('',#11282,#7702,#7703);
#6075=AXIS2_PLACEMENT_3D('',#11283,#7704,#7705);
#6076=AXIS2_PLACEMENT_3D('',#11284,#7706,#7707);
#6077=AXIS2_PLACEMENT_3D('',#11285,#7708,#7709);
#6078=AXIS2_PLACEMENT_3D('',#11287,#7710,#7711);
#6079=AXIS2_PLACEMENT_3D('',#11289,#7712,#7713);
#6080=AXIS2_PLACEMENT_3D('',#11290,#7714,#7715);
#6081=AXIS2_PLACEMENT_3D('',#11292,#7716,#7717);
#6082=AXIS2_PLACEMENT_3D('',#11294,#7718,#7719);
#6083=AXIS2_PLACEMENT_3D('',#11295,#7720,#7721);
#6084=AXIS2_PLACEMENT_3D('',#11296,#7722,#7723);
#6085=AXIS2_PLACEMENT_3D('',#11299,#7725,#7726);
#6086=AXIS2_PLACEMENT_3D('',#11300,#7727,#7728);
#6087=AXIS2_PLACEMENT_3D('',#11301,#7729,#7730);
#6088=AXIS2_PLACEMENT_3D('',#11310,#7735,#7736);
#6089=AXIS2_PLACEMENT_3D('',#11316,#7740,#7741);
#6090=AXIS2_PLACEMENT_3D('',#11322,#7745,#7746);
#6091=AXIS2_PLACEMENT_3D('',#11328,#7750,#7751);
#6092=AXIS2_PLACEMENT_3D('',#11334,#7755,#7756);
#6093=AXIS2_PLACEMENT_3D('',#11337,#7759,#7760);
#6094=AXIS2_PLACEMENT_3D('',#11338,#7761,#7762);
#6095=AXIS2_PLACEMENT_3D('',#11340,#7763,#7764);
#6096=AXIS2_PLACEMENT_3D('',#11342,#7766,#7767);
#6097=AXIS2_PLACEMENT_3D('',#11343,#7768,#7769);
#6098=AXIS2_PLACEMENT_3D('',#11344,#7770,#7771);
#6099=AXIS2_PLACEMENT_3D('',#11345,#7772,#7773);
#6100=AXIS2_PLACEMENT_3D('',#11346,#7774,#7775);
#6101=AXIS2_PLACEMENT_3D('',#11347,#7776,#7777);
#6102=AXIS2_PLACEMENT_3D('',#11348,#7778,#7779);
#6103=AXIS2_PLACEMENT_3D('',#11349,#7780,#7781);
#6104=AXIS2_PLACEMENT_3D('',#11350,#7782,#7783);
#6105=AXIS2_PLACEMENT_3D('',#11351,#7784,#7785);
#6106=AXIS2_PLACEMENT_3D('',#11352,#7786,#7787);
#6107=AXIS2_PLACEMENT_3D('',#11353,#7788,#7789);
#6108=AXIS2_PLACEMENT_3D('',#11354,#7790,#7791);
#6109=AXIS2_PLACEMENT_3D('',#11355,#7792,#7793);
#6110=DIRECTION('axis',(0.,0.,1.));
#6111=DIRECTION('refdir',(1.,0.,0.));
#6112=DIRECTION('axis',(0.,0.,1.));
#6113=DIRECTION('refdir',(1.,0.,0.));
#6114=DIRECTION('center_axis',(-1.,0.,0.));
#6115=DIRECTION('ref_axis',(0.,1.,3.83915447951421E-33));
#6116=DIRECTION('',(0.,1.,1.22464679914735E-16));
#6117=DIRECTION('',(0.,0.,-1.));
#6118=DIRECTION('',(0.,1.,3.83915447951421E-33));
#6119=DIRECTION('',(0.,0.,-1.));
#6120=DIRECTION('center_axis',(0.,0.,-1.));
#6121=DIRECTION('ref_axis',(-0.717326861318586,0.696736803987579,0.));
#6122=DIRECTION('center_axis',(0.,1.22464679914735E-16,-1.));
#6123=DIRECTION('ref_axis',(-0.717326861318586,0.696736803987579,0.));
#6124=DIRECTION('',(0.,0.,-1.));
#6125=DIRECTION('center_axis',(1.55523680250478E-33,-1.51059548673417E-33,
-1.));
#6126=DIRECTION('ref_axis',(-0.717326861318586,0.696736803987579,-2.16810060569314E-33));
#6127=DIRECTION('center_axis',(-1.,0.,0.));
#6128=DIRECTION('ref_axis',(0.,1.,0.));
#6129=DIRECTION('',(0.,1.,1.22464679914735E-16));
#6130=DIRECTION('',(0.,0.,-1.));
#6131=DIRECTION('',(0.,1.,0.));
#6132=DIRECTION('center_axis',(0.,0.,-1.));
#6133=DIRECTION('ref_axis',(-1.,0.,0.));
#6134=DIRECTION('center_axis',(0.,1.22464679914735E-16,-1.));
#6135=DIRECTION('ref_axis',(-1.,0.,0.));
#6136=DIRECTION('',(0.,0.,-1.));
#6137=DIRECTION('center_axis',(0.,0.,-1.));
#6138=DIRECTION('ref_axis',(-1.,0.,0.));
#6139=DIRECTION('center_axis',(1.,1.87772095759185E-15,0.));
#6140=DIRECTION('ref_axis',(1.87772095759185E-15,-1.,-8.60989605595408E-34));
#6141=DIRECTION('',(1.87772095759185E-15,-1.,-1.22464679914735E-16));
#6142=DIRECTION('',(0.,0.,-1.));
#6143=DIRECTION('',(1.87772095759185E-15,-1.,-8.60989605595408E-34));
#6144=DIRECTION('center_axis',(0.,0.,-1.));
#6145=DIRECTION('ref_axis',(0.747636447008101,-0.664108231469166,0.));
#6146=DIRECTION('center_axis',(0.,1.22464679914735E-16,-1.));
#6147=DIRECTION('ref_axis',(0.747636447008101,-0.664108231469166,0.));
#6148=DIRECTION('',(0.,0.,-1.));
#6149=DIRECTION('center_axis',(3.84526517546801E-34,-3.41566046629928E-34,
-1.));
#6150=DIRECTION('ref_axis',(0.747636447008101,-0.664108231469166,5.14322862516405E-34));
#6151=DIRECTION('center_axis',(1.,9.38860478795921E-16,0.));
#6152=DIRECTION('ref_axis',(9.38860478795921E-16,-1.,2.05736781630139E-32));
#6153=DIRECTION('',(9.38860478795921E-16,-1.,-1.22464679914735E-16));
#6154=DIRECTION('',(0.,0.,-1.));
#6155=DIRECTION('',(9.38860478795921E-16,-1.,2.05736781630139E-32));
#6156=DIRECTION('center_axis',(0.,0.,-1.));
#6157=DIRECTION('ref_axis',(1.,0.,0.));
#6158=DIRECTION('center_axis',(0.,1.22464679914735E-16,-1.));
#6159=DIRECTION('ref_axis',(1.,0.,0.));
#6160=DIRECTION('center_axis',(0.,0.,-1.));
#6161=DIRECTION('ref_axis',(1.,0.,0.));
#6162=DIRECTION('center_axis',(1.98620985225205E-15,-1.,0.));
#6163=DIRECTION('ref_axis',(-1.,-1.98620985225205E-15,0.));
#6164=DIRECTION('',(-1.,-1.98620985225205E-15,-2.43240553799541E-31));
#6165=DIRECTION('',(0.,0.,-1.));
#6166=DIRECTION('',(-1.,-1.98620985225205E-15,0.));
#6167=DIRECTION('',(0.,0.,-1.));
#6168=DIRECTION('center_axis',(0.,0.,-1.));
#6169=DIRECTION('ref_axis',(-0.696736803987579,-0.717326861318586,0.));
#6170=DIRECTION('center_axis',(0.,1.22464679914735E-16,-1.));
#6171=DIRECTION('ref_axis',(-0.696736803987579,-0.717326861318586,0.));
#6172=DIRECTION('',(0.,0.,-1.));
#6173=DIRECTION('center_axis',(6.92366496631146E-48,7.12827402066476E-48,
-1.));
#6174=DIRECTION('ref_axis',(-0.696736803987579,-0.717326861318586,-9.93727463037089E-48));
#6175=DIRECTION('center_axis',(0.,-1.,0.));
#6176=DIRECTION('ref_axis',(-1.,0.,-2.30940147376294E-32));
#6177=DIRECTION('',(-1.,0.,0.));
#6178=DIRECTION('',(0.,0.,-1.));
#6179=DIRECTION('',(-1.,0.,-2.30940147376294E-32));
#6180=DIRECTION('center_axis',(0.,0.,-1.));
#6181=DIRECTION('ref_axis',(-1.33992434006485E-15,-1.,0.));
#6182=DIRECTION('center_axis',(0.,1.22464679914735E-16,-1.));
#6183=DIRECTION('ref_axis',(-1.33992434006485E-15,-1.,0.));
#6184=DIRECTION('',(0.,0.,-1.));
#6185=DIRECTION('center_axis',(0.,0.,-1.));
#6186=DIRECTION('ref_axis',(-1.33992434006485E-15,-1.,0.));
#6187=DIRECTION('center_axis',(7.51088383036733E-15,1.,0.));
#6188=DIRECTION('ref_axis',(1.,-7.51088383036733E-15,-2.05736781630138E-32));
#6189=DIRECTION('',(1.,-7.51088383036733E-15,-9.19817984162697E-31));
#6190=DIRECTION('',(0.,0.,-1.));
#6191=DIRECTION('',(1.,-7.51088383036733E-15,-2.05736781630138E-32));
#6192=DIRECTION('center_axis',(0.,0.,-1.));
#6193=DIRECTION('ref_axis',(0.664108231469163,0.747636447008103,0.));
#6194=DIRECTION('center_axis',(0.,1.22464679914735E-16,-1.));
#6195=DIRECTION('ref_axis',(0.664108231469163,0.747636447008103,0.));
#6196=DIRECTION('',(0.,0.,-1.));
#6197=DIRECTION('center_axis',(8.16185220949039E-33,9.18840920464028E-33,
-1.));
#6198=DIRECTION('ref_axis',(0.664108231469163,0.747636447008103,1.22899428477711E-32));
#6199=DIRECTION('center_axis',(-3.75544191518368E-15,1.,0.));
#6200=DIRECTION('ref_axis',(1.,3.75544191518368E-15,8.60989605595486E-34));
#6201=DIRECTION('',(1.,3.75544191518368E-15,4.5990899208135E-31));
#6202=DIRECTION('',(0.,0.,-1.));
#6203=DIRECTION('',(1.,3.75544191518368E-15,8.60989605595486E-34));
#6204=DIRECTION('center_axis',(0.,0.,-1.));
#6205=DIRECTION('ref_axis',(0.,1.,0.));
#6206=DIRECTION('center_axis',(0.,1.22464679914735E-16,-1.));
#6207=DIRECTION('ref_axis',(0.,1.,0.));
#6208=DIRECTION('center_axis',(0.,0.,-1.));
#6209=DIRECTION('ref_axis',(0.,1.,0.));
#6210=DIRECTION('center_axis',(1.,0.,0.));
#6211=DIRECTION('ref_axis',(0.,-1.,2.50419113937346E-32));
#6212=DIRECTION('',(0.,-1.,-1.22464679914735E-16));
#6213=DIRECTION('',(0.,0.,-1.));
#6214=DIRECTION('',(0.,-1.,2.50419113937346E-32));
#6215=DIRECTION('',(0.,0.,-1.));
#6216=DIRECTION('center_axis',(0.,0.,-1.));
#6217=DIRECTION('ref_axis',(1.,0.,0.));
#6218=DIRECTION('center_axis',(0.,1.22464679914735E-16,-1.));
#6219=DIRECTION('ref_axis',(1.,0.,0.));
#6220=DIRECTION('',(0.,0.,-1.));
#6221=DIRECTION('center_axis',(0.,0.,-1.));
#6222=DIRECTION('ref_axis',(1.,0.,0.));
#6223=DIRECTION('center_axis',(-1.,0.,0.));
#6224=DIRECTION('ref_axis',(0.,1.,-8.04212236896447E-32));
#6225=DIRECTION('',(0.,1.,1.22464679914735E-16));
#6226=DIRECTION('',(0.,0.,-1.));
#6227=DIRECTION('',(0.,1.,-8.04212236896447E-32));
#6228=DIRECTION('center_axis',(0.,0.,-1.));
#6229=DIRECTION('ref_axis',(-0.732481654163345,0.680786770078657,0.));
#6230=DIRECTION('center_axis',(0.,1.22464679914735E-16,-1.));
#6231=DIRECTION('ref_axis',(-0.732481654163345,0.680786770078657,0.));
#6232=DIRECTION('',(0.,0.,-1.));
#6233=DIRECTION('center_axis',(0.,0.,-1.));
#6234=DIRECTION('ref_axis',(-0.732481654163345,0.680786770078657,0.));
#6235=DIRECTION('center_axis',(-1.,0.,0.));
#6236=DIRECTION('ref_axis',(0.,1.,0.));
#6237=DIRECTION('',(0.,1.,1.22464679914735E-16));
#6238=DIRECTION('',(0.,0.,-1.));
#6239=DIRECTION('',(0.,1.,0.));
#6240=DIRECTION('center_axis',(0.,0.,-1.));
#6241=DIRECTION('ref_axis',(-1.,3.0626842058625E-15,0.));
#6242=DIRECTION('center_axis',(0.,1.22464679914735E-16,-1.));
#6243=DIRECTION('ref_axis',(-1.,3.0626842058625E-15,0.));
#6244=DIRECTION('',(0.,0.,-1.));
#6245=DIRECTION('center_axis',(0.,0.,-1.));
#6246=DIRECTION('ref_axis',(-1.,3.0626842058625E-15,0.));
#6247=DIRECTION('center_axis',(1.,0.,0.));
#6248=DIRECTION('ref_axis',(0.,-1.,7.62844485451842E-49));
#6249=DIRECTION('',(0.,-1.,-1.22464679914735E-16));
#6250=DIRECTION('',(0.,0.,-1.));
#6251=DIRECTION('',(0.,-1.,7.62844485451842E-49));
#6252=DIRECTION('center_axis',(0.,0.,-1.));
#6253=DIRECTION('ref_axis',(0.732481654163344,-0.680786770078658,0.));
#6254=DIRECTION('center_axis',(0.,1.22464679914735E-16,-1.));
#6255=DIRECTION('ref_axis',(0.732481654163344,-0.680786770078658,0.));
#6256=DIRECTION('center_axis',(-3.24468512908471E-49,3.01569151445155E-49,
-1.));
#6257=DIRECTION('ref_axis',(0.732481654163344,-0.680786770078658,-4.42971521626826E-49));
#6258=DIRECTION('center_axis',(0.,1.,0.));
#6259=DIRECTION('ref_axis',(1.,0.,0.));
#6260=DIRECTION('',(1.,0.,0.));
#6261=DIRECTION('',(0.,0.,-1.));
#6262=DIRECTION('',(1.,0.,0.));
#6263=DIRECTION('',(0.,0.,-1.));
#6264=DIRECTION('center_axis',(0.,0.,-1.));
#6265=DIRECTION('ref_axis',(0.680786770078658,0.732481654163344,0.));
#6266=DIRECTION('center_axis',(0.,1.22464679914735E-16,-1.));
#6267=DIRECTION('ref_axis',(0.680786770078658,0.732481654163344,0.));
#6268=DIRECTION('',(0.,0.,-1.));
#6269=DIRECTION('center_axis',(0.,0.,-1.));
#6270=DIRECTION('ref_axis',(0.680786770078658,0.732481654163344,0.));
#6271=DIRECTION('center_axis',(0.,1.,0.));
#6272=DIRECTION('ref_axis',(1.,0.,0.));
#6273=DIRECTION('',(1.,0.,0.));
#6274=DIRECTION('',(0.,0.,-1.));
#6275=DIRECTION('',(1.,0.,0.));
#6276=DIRECTION('center_axis',(0.,0.,-1.));
#6277=DIRECTION('ref_axis',(0.,1.,0.));
#6278=DIRECTION('center_axis',(0.,1.22464679914735E-16,-1.));
#6279=DIRECTION('ref_axis',(0.,1.,0.));
#6280=DIRECTION('',(0.,0.,-1.));
#6281=DIRECTION('center_axis',(0.,0.,-1.));
#6282=DIRECTION('ref_axis',(0.,1.,0.));
#6283=DIRECTION('center_axis',(0.,-1.,0.));
#6284=DIRECTION('ref_axis',(-1.,0.,-6.35647172290725E-34));
#6285=DIRECTION('',(-1.,0.,0.));
#6286=DIRECTION('',(0.,0.,-1.));
#6287=DIRECTION('',(-1.,0.,-6.35647172290725E-34));
#6288=DIRECTION('center_axis',(0.,0.,-1.));
#6289=DIRECTION('ref_axis',(-0.680786770078657,-0.732481654163345,0.));
#6290=DIRECTION('center_axis',(0.,1.22464679914735E-16,-1.));
#6291=DIRECTION('ref_axis',(-0.680786770078657,-0.732481654163345,0.));
#6292=DIRECTION('',(0.,0.,-1.));
#6293=DIRECTION('center_axis',(-2.51285264587953E-34,-2.70366367799702E-34,
-1.));
#6294=DIRECTION('ref_axis',(-0.680786770078657,-0.732481654163345,3.69110087963254E-34));
#6295=DIRECTION('center_axis',(0.,-1.,0.));
#6296=DIRECTION('ref_axis',(-1.,0.,0.));
#6297=DIRECTION('',(-1.,0.,0.));
#6298=DIRECTION('',(0.,0.,-1.));
#6299=DIRECTION('',(-1.,0.,0.));
#6300=DIRECTION('center_axis',(0.,0.,-1.));
#6301=DIRECTION('ref_axis',(-1.91417762866406E-16,-1.,0.));
#6302=DIRECTION('center_axis',(0.,1.22464679914735E-16,-1.));
#6303=DIRECTION('ref_axis',(-1.91417762866406E-16,-1.,0.));
#6304=DIRECTION('center_axis',(0.,0.,-1.));
#6305=DIRECTION('ref_axis',(-1.91417762866406E-16,-1.,0.));
#6306=DIRECTION('center_axis',(0.,1.22464679914735E-16,-1.));
#6307=DIRECTION('ref_axis',(1.,0.,0.));
#6308=DIRECTION('center_axis',(0.,-1.22464679914735E-16,1.));
#6309=DIRECTION('ref_axis',(1.,0.,0.));
#6310=DIRECTION('',(0.,-1.22464679914735E-16,1.));
#6311=DIRECTION('center_axis',(-3.84526517546801E-34,3.41566046629928E-34,
1.));
#6312=DIRECTION('ref_axis',(1.,0.,0.));
#6313=DIRECTION('center_axis',(0.,-1.22464679914735E-16,1.));
#6314=DIRECTION('ref_axis',(-2.22044604925031E-16,1.,1.22464679914735E-16));
#6315=DIRECTION('center_axis',(0.,1.22464679914735E-16,-1.));
#6316=DIRECTION('ref_axis',(-2.22044604925031E-16,1.,1.22464679914735E-16));
#6317=DIRECTION('',(0.,-1.22464679914735E-16,1.));
#6318=DIRECTION('center_axis',(0.,0.,1.));
#6319=DIRECTION('ref_axis',(-2.22044604925031E-16,1.,1.22464679914735E-16));
#6320=DIRECTION('center_axis',(0.,1.22464679914735E-16,-1.));
#6321=DIRECTION('ref_axis',(-2.22044604925031E-16,1.,1.22464679914735E-16));
#6322=DIRECTION('center_axis',(0.,1.22464679914735E-16,-1.));
#6323=DIRECTION('ref_axis',(-2.22044604925031E-16,1.,1.22464679914735E-16));
#6324=DIRECTION('',(-0.707098477694133,0.00342678313306322,0.707106781186547));
#6325=DIRECTION('center_axis',(0.,-1.22464679914735E-16,1.));
#6326=DIRECTION('ref_axis',(-2.22044604925031E-16,1.,1.22464679914735E-16));
#6327=DIRECTION('center_axis',(0.,-1.22464679914735E-16,1.));
#6328=DIRECTION('ref_axis',(-0.999997064267793,0.00242310870464513,2.96745231912974E-19));
#6329=DIRECTION('',(-0.707106781186563,-8.65956056235474E-17,0.707106781186532));
#6330=DIRECTION('center_axis',(0.,1.22464679914735E-16,-1.));
#6331=DIRECTION('ref_axis',(-0.999997064267793,0.00242310870464512,2.96745231912974E-19));
#6332=DIRECTION('center_axis',(0.,-1.22464679914735E-16,1.));
#6333=DIRECTION('ref_axis',(-0.999997064267794,0.00242310870464513,2.96745231912974E-19));
#6334=DIRECTION('center_axis',(-0.707106781186548,-7.04136402448282E-17,
-0.707106781186548));
#6335=DIRECTION('ref_axis',(0.707106781186548,8.65956056235493E-17,-0.707106781186548));
#6336=DIRECTION('',(-0.707106781186547,-8.65956056235493E-17,0.707106781186547));
#6337=DIRECTION('',(-2.22044604925031E-16,1.,1.22464679914735E-16));
#6338=DIRECTION('',(2.22044604925031E-16,-1.,-1.22464679914735E-16));
#6339=DIRECTION('center_axis',(0.,-1.22464679914735E-16,1.));
#6340=DIRECTION('ref_axis',(-1.,-1.20644235342523E-14,-1.47746576647801E-30));
#6341=DIRECTION('',(-0.70568734200296,-0.0447814173156507,0.707106781186547));
#6342=DIRECTION('center_axis',(0.,1.22464679914735E-16,-1.));
#6343=DIRECTION('ref_axis',(-1.,-1.20644235342523E-14,-1.47746576647801E-30));
#6344=DIRECTION('center_axis',(0.,-1.22464679914735E-16,1.));
#6345=DIRECTION('ref_axis',(-1.,-1.20644235342523E-14,-1.47746576647801E-30));
#6346=DIRECTION('center_axis',(-0.705687342002958,-0.0447814173156751,-0.707106781186548));
#6347=DIRECTION('ref_axis',(0.707816856590716,8.65085590544045E-17,-0.706395992008758));
#6348=DIRECTION('',(-0.705687342002958,-0.0447814173156759,0.707106781186547));
#6349=DIRECTION('',(-0.0633304877101172,0.997992609855604,1.22218845523238E-16));
#6350=DIRECTION('',(0.0633304877101172,-0.997992609855604,-1.22218845523238E-16));
#6351=DIRECTION('center_axis',(0.,-1.22464679914735E-16,1.));
#6352=DIRECTION('ref_axis',(-0.997992609855603,-0.0633304877101176,-7.75574790626363E-18));
#6353=DIRECTION('',(-0.495178732794061,-0.504775219863721,0.707106781186547));
#6354=DIRECTION('center_axis',(0.,1.22464679914735E-16,-1.));
#6355=DIRECTION('ref_axis',(-0.997992609855603,-0.0633304877101176,-7.75574790626363E-18));
#6356=DIRECTION('center_axis',(0.,-1.22464679914735E-16,1.));
#6357=DIRECTION('ref_axis',(-0.997992609855603,-0.0633304877101176,-7.75574790626363E-18));
#6358=DIRECTION('center_axis',(-0.495178732794066,-0.504775219863718,-0.707106781186546));
#6359=DIRECTION('ref_axis',(0.819120891857568,7.02483028577243E-17,-0.573620924062627));
#6360=DIRECTION('',(-0.495178732794064,-0.504775219863716,0.707106781186549));
#6361=DIRECTION('',(-0.71385996188113,0.700288479716089,8.57606045164075E-17));
#6362=DIRECTION('',(0.71385996188113,-0.700288479716089,-8.57606045164075E-17));
#6363=DIRECTION('center_axis',(0.,-1.22464679914735E-16,1.));
#6364=DIRECTION('ref_axis',(-0.700288479716085,-0.713859961881135,-8.74226317357183E-17));
#6365=DIRECTION('',(-4.71027737605131E-15,-0.707106781186549,0.707106781186546));
#6366=DIRECTION('center_axis',(0.,1.22464679914735E-16,-1.));
#6367=DIRECTION('ref_axis',(-0.700288479716085,-0.713859961881135,-8.74226317357183E-17));
#6368=DIRECTION('center_axis',(0.,-1.22464679914735E-16,1.));
#6369=DIRECTION('ref_axis',(-0.700288479716085,-0.713859961881135,-8.74226317357183E-17));
#6370=DIRECTION('center_axis',(1.57009245868378E-16,-0.707106781186549,
-0.707106781186546));
#6371=DIRECTION('ref_axis',(1.,-2.71926214689379E-32,2.22044604925032E-16));
#6372=DIRECTION('',(0.,-0.707106781186546,0.707106781186549));
#6373=DIRECTION('',(-1.,-2.22044604925031E-16,-2.71926214689378E-32));
#6374=DIRECTION('',(1.,2.22044604925031E-16,2.71926214689378E-32));
#6375=DIRECTION('center_axis',(0.,-1.22464679914735E-16,1.));
#6376=DIRECTION('ref_axis',(-1.44328993201271E-15,-1.,-1.22464679914735E-16));
#6377=DIRECTION('',(0.501258447848715,-0.498738376767117,0.707106781186546));
#6378=DIRECTION('center_axis',(0.,1.22464679914735E-16,-1.));
#6379=DIRECTION('ref_axis',(-1.44328993201271E-15,-1.,-1.22464679914735E-16));
#6380=DIRECTION('center_axis',(0.,-1.22464679914735E-16,1.));
#6381=DIRECTION('ref_axis',(-1.44328993201271E-15,-1.,-1.22464679914735E-16));
#6382=DIRECTION('center_axis',(0.501258447848716,-0.498738376767119,-0.707106781186545));
#6383=DIRECTION('ref_axis',(0.815811569646784,-7.08235047989531E-17,0.578317804351942));
#6384=DIRECTION('',(0.501258447848714,-0.498738376767113,0.70710678118655));
#6385=DIRECTION('',(-0.705322576499999,-0.708886495201738,-8.68135577307594E-17));
#6386=DIRECTION('',(0.705322576499999,0.708886495201738,8.68135577307594E-17));
#6387=DIRECTION('center_axis',(0.,-1.22464679914735E-16,1.));
#6388=DIRECTION('ref_axis',(0.708886495201743,-0.705322576499993,-8.63771035677081E-17));
#6389=DIRECTION('',(0.702660115090392,-0.0791755180668618,0.707106781186548));
#6390=DIRECTION('center_axis',(0.,1.22464679914735E-16,-1.));
#6391=DIRECTION('ref_axis',(0.708886495201743,-0.705322576499994,-8.63771035677081E-17));
#6392=DIRECTION('center_axis',(0.,-1.22464679914735E-16,1.));
#6393=DIRECTION('ref_axis',(0.708886495201743,-0.705322576499994,-8.63771035677081E-17));
#6394=DIRECTION('center_axis',(0.702660115090393,-0.0791755180668588,-0.707106781186547));
#6395=DIRECTION('ref_axis',(0.709333598508651,-8.63220376296547E-17,0.704872928992714));
#6396=DIRECTION('',(0.702660115090393,-0.0791755180668555,0.707106781186548));
#6397=DIRECTION('',(-0.111971091458068,-0.993711464499474,-1.21694556427531E-16));
#6398=DIRECTION('',(0.111971091458068,0.993711464499474,1.21694556427531E-16));
#6399=DIRECTION('center_axis',(0.,-1.22464679914735E-16,1.));
#6400=DIRECTION('ref_axis',(0.993711464499475,-0.111971091458059,-1.37125038751148E-17));
#6401=DIRECTION('',(0.707106781186547,-1.26473352750937E-14,0.707106781186548));
#6402=DIRECTION('center_axis',(0.,1.22464679914735E-16,-1.));
#6403=DIRECTION('ref_axis',(0.993711464499475,-0.111971091458059,-1.37125038751148E-17));
#6404=DIRECTION('center_axis',(0.,-1.22464679914735E-16,1.));
#6405=DIRECTION('ref_axis',(0.993711464499475,-0.111971091458059,-1.37125038751148E-17));
#6406=DIRECTION('center_axis',(0.707106781186548,2.43045314947538E-16,-0.707106781186547));
#6407=DIRECTION('ref_axis',(0.707106781186547,-8.65956056235494E-17,0.707106781186548));
#6408=DIRECTION('',(0.707106781186547,-8.65956056235494E-17,0.707106781186548));
#6409=DIRECTION('',(2.21253300755314E-16,-1.,-1.22464679914735E-16));
#6410=DIRECTION('',(-2.21253300755314E-16,1.,1.22464679914735E-16));
#6411=DIRECTION('center_axis',(0.,-1.22464679914735E-16,1.));
#6412=DIRECTION('ref_axis',(1.,3.92278802034127E-15,4.80402979284452E-31));
#6413=DIRECTION('',(0.701854257103615,0.0860267504066733,0.707106781186548));
#6414=DIRECTION('center_axis',(0.,1.22464679914735E-16,-1.));
#6415=DIRECTION('ref_axis',(1.,3.92278802034127E-15,4.80402979284452E-31));
#6416=DIRECTION('center_axis',(0.,-1.22464679914735E-16,1.));
#6417=DIRECTION('ref_axis',(1.,3.92278802034127E-15,4.80402979284452E-31));
#6418=DIRECTION('center_axis',(0.701854257103617,0.0860267504066795,-0.707106781186545));
#6419=DIRECTION('ref_axis',(0.709737901988185,-8.62721828028444E-17,0.704465833437938));
#6420=DIRECTION('',(0.701854257103612,0.0860267504066774,0.70710678118655));
#6421=DIRECTION('',(0.121660197152011,-0.992571809205225,-1.21554988906708E-16));
#6422=DIRECTION('',(-0.121660197152011,0.992571809205225,1.21554988906708E-16));
#6423=DIRECTION('center_axis',(0.,-1.22464679914735E-16,1.));
#6424=DIRECTION('ref_axis',(0.12166019715201,0.992571809205225,1.21554988906708E-16));
#6425=DIRECTION('center_axis',(0.,-1.22464679914735E-16,1.));
#6426=DIRECTION('ref_axis',(0.12166019715201,0.992571809205225,1.21554988906708E-16));
#6427=DIRECTION('',(0.0860267504066787,0.701854257103615,0.707106781186548));
#6428=DIRECTION('center_axis',(0.,1.22464679914735E-16,-1.));
#6429=DIRECTION('ref_axis',(0.12166019715201,0.992571809205225,1.21554988906708E-16));
#6430=DIRECTION('center_axis',(0.0860267504066789,0.701854257103615,-0.707106781186548));
#6431=DIRECTION('ref_axis',(0.992680551218392,-1.4790024070839E-17,0.120769711570196));
#6432=DIRECTION('',(-0.992571809205225,0.121660197152011,1.48990771025846E-17));
#6433=DIRECTION('',(0.086026750406678,0.701854257103615,0.707106781186548));
#6434=DIRECTION('',(0.992571809205225,-0.121660197152011,-1.48990771025846E-17));
#6435=DIRECTION('center_axis',(0.,-1.22464679914735E-16,1.));
#6436=DIRECTION('ref_axis',(3.70074341541624E-15,1.,1.22464679914735E-16));
#6437=DIRECTION('center_axis',(0.,-1.22464679914735E-16,1.));
#6438=DIRECTION('ref_axis',(3.70074341541624E-15,1.,1.22464679914735E-16));
#6439=DIRECTION('',(3.14018491736755E-15,0.707106781186547,0.707106781186548));
#6440=DIRECTION('center_axis',(0.,1.22464679914735E-16,-1.));
#6441=DIRECTION('ref_axis',(3.70074341541624E-15,1.,1.22464679914735E-16));
#6442=DIRECTION('center_axis',(-5.59536544388552E-19,0.707106781186548,
-0.707106781186547));
#6443=DIRECTION('ref_axis',(1.,9.69068118596694E-35,-7.91304169717666E-19));
#6444=DIRECTION('',(-1.,-7.91304169717665E-19,-9.69068118596693E-35));
#6445=DIRECTION('',(0.,0.707106781186547,0.707106781186548));
#6446=DIRECTION('',(1.,7.91304169717665E-19,9.69068118596693E-35));
#6447=DIRECTION('center_axis',(0.,-1.22464679914735E-16,1.));
#6448=DIRECTION('ref_axis',(-0.111971091458059,0.993711464499475,1.21694556427531E-16));
#6449=DIRECTION('center_axis',(0.,-1.22464679914735E-16,1.));
#6450=DIRECTION('ref_axis',(-0.111971091458059,0.993711464499475,1.21694556427531E-16));
#6451=DIRECTION('',(-0.0791755180668554,0.702660115090393,0.707106781186548));
#6452=DIRECTION('center_axis',(0.,1.22464679914735E-16,-1.));
#6453=DIRECTION('ref_axis',(-0.111971091458059,0.993711464499475,1.21694556427531E-16));
#6454=DIRECTION('center_axis',(-0.0791755180668589,0.702660115090393,-0.707106781186548));
#6455=DIRECTION('ref_axis',(0.993789574232718,1.36273433877159E-17,-0.111275703306486));
#6456=DIRECTION('',(-0.993711464499474,-0.111971091458068,-1.37125038751159E-17));
#6457=DIRECTION('',(-0.0791755180668615,0.702660115090393,0.707106781186547));
#6458=DIRECTION('',(0.993711464499474,0.111971091458068,1.37125038751159E-17));
#6459=DIRECTION('center_axis',(0.,-1.22464679914735E-16,1.));
#6460=DIRECTION('ref_axis',(-0.705322576499994,0.708886495201743,8.681355773076E-17));
#6461=DIRECTION('center_axis',(0.,-1.22464679914735E-16,1.));
#6462=DIRECTION('ref_axis',(-0.705322576499994,0.708886495201743,8.681355773076E-17));
#6463=DIRECTION('',(-0.498738376767112,0.501258447848717,0.707106781186548));
#6464=DIRECTION('center_axis',(0.,1.22464679914735E-16,-1.));
#6465=DIRECTION('ref_axis',(-0.705322576499994,0.708886495201743,8.681355773076E-17));
#6466=DIRECTION('center_axis',(-0.498738376767117,0.501258447848714,-0.707106781186547));
#6467=DIRECTION('ref_axis',(0.817183320658714,7.05859283223419E-17,-0.576377845199829));
#6468=DIRECTION('',(-0.708886495201738,-0.705322576499999,-8.63771035677088E-17));
#6469=DIRECTION('',(-0.498738376767117,0.501258447848713,0.707106781186547));
#6470=DIRECTION('',(0.708886495201738,0.705322576499999,8.63771035677088E-17));
#6471=DIRECTION('center_axis',(0.,-1.22464679914735E-16,1.));
#6472=DIRECTION('ref_axis',(-1.,-1.66533453693774E-15,-2.03944661017034E-31));
#6473=DIRECTION('center_axis',(0.,-1.22464679914735E-16,1.));
#6474=DIRECTION('ref_axis',(-1.,-1.66533453693774E-15,-2.03944661017034E-31));
#6475=DIRECTION('',(-0.707106781186549,-1.65668806430732E-15,0.707106781186546));
#6476=DIRECTION('center_axis',(0.,1.22464679914735E-16,-1.));
#6477=DIRECTION('ref_axis',(-1.,-1.66533453693774E-15,-2.03944661017034E-31));
#6478=DIRECTION('center_axis',(-0.707106781186549,8.65956056235491E-17,
-0.707106781186546));
#6479=DIRECTION('ref_axis',(0.707106781186546,8.65956056235495E-17,-0.707106781186549));
#6480=DIRECTION('',(0.,-1.,-1.22464679914735E-16));
#6481=DIRECTION('',(-0.707106781186546,-8.65956056235495E-17,0.707106781186549));
#6482=DIRECTION('',(0.,1.,1.22464679914735E-16));
#6483=DIRECTION('center_axis',(0.,-1.22464679914735E-16,1.));
#6484=DIRECTION('ref_axis',(-0.713859961881135,-0.700288479716084,-8.57606045164069E-17));
#6485=DIRECTION('center_axis',(0.,-1.22464679914735E-16,1.));
#6486=DIRECTION('ref_axis',(-0.713859961881135,-0.700288479716085,-8.57606045164069E-17));
#6487=DIRECTION('',(-0.504775219863721,-0.495178732794061,0.707106781186547));
#6488=DIRECTION('center_axis',(0.,1.22464679914735E-16,-1.));
#6489=DIRECTION('ref_axis',(-0.713859961881135,-0.700288479716085,-8.57606045164069E-17));
#6490=DIRECTION('center_axis',(-0.504775219863718,-0.495178732794066,-0.707106781186546));
#6491=DIRECTION('ref_axis',(0.813897332858798,7.11530468011979E-17,-0.581008719009737));
#6492=DIRECTION('',(0.700288479716089,-0.71385996188113,-8.74226317357177E-17));
#6493=DIRECTION('',(-0.504775219863716,-0.495178732794063,0.70710678118655));
#6494=DIRECTION('',(-0.700288479716089,0.71385996188113,8.74226317357177E-17));
#6495=DIRECTION('center_axis',(0.,-1.22464679914735E-16,1.));
#6496=DIRECTION('ref_axis',(-0.0633304877101173,-0.997992609855603,-1.22218845523238E-16));
#6497=DIRECTION('center_axis',(0.,-1.22464679914735E-16,1.));
#6498=DIRECTION('ref_axis',(-0.0633304877101173,-0.997992609855603,-1.22218845523238E-16));
#6499=DIRECTION('',(-0.0447814173156758,-0.705687342002959,0.707106781186547));
#6500=DIRECTION('center_axis',(0.,1.22464679914735E-16,-1.));
#6501=DIRECTION('ref_axis',(-0.0633304877101173,-0.997992609855604,-1.22218845523238E-16));
#6502=DIRECTION('center_axis',(-0.044781417315675,-0.705687342002958,-0.707106781186548));
#6503=DIRECTION('ref_axis',(0.998000636867369,7.74024134983379E-18,-0.0632038670678178));
#6504=DIRECTION('',(0.997992609855604,-0.063330487710117,-7.75574790626356E-18));
#6505=DIRECTION('',(-0.0447814173156758,-0.705687342002958,0.707106781186547));
#6506=DIRECTION('',(-0.997992609855604,0.063330487710117,7.75574790626356E-18));
#6507=DIRECTION('center_axis',(0.,-1.22464679914735E-16,1.));
#6508=DIRECTION('ref_axis',(-1.18423789293273E-14,-1.,-1.22464679914735E-16));
#6509=DIRECTION('center_axis',(0.,-1.22464679914735E-16,1.));
#6510=DIRECTION('ref_axis',(-1.18423789293273E-14,-1.,-1.22464679914735E-16));
#6511=DIRECTION('',(-6.28036983473509E-15,-0.707106781186548,0.707106781186547));
#6512=DIRECTION('center_axis',(0.,1.22464679914735E-16,-1.));
#6513=DIRECTION('ref_axis',(-1.18423789293273E-14,-1.,-1.22464679914735E-16));
#6514=DIRECTION('center_axis',(0.,-0.707106781186547,-0.707106781186548));
#6515=DIRECTION('ref_axis',(1.,0.,0.));
#6516=DIRECTION('',(1.,0.,0.));
#6517=DIRECTION('',(0.,-0.707106781186554,0.707106781186541));
#6518=DIRECTION('',(-1.,0.,0.));
#6519=DIRECTION('center_axis',(0.,-1.22464679914735E-16,1.));
#6520=DIRECTION('ref_axis',(0.00242310870467221,-0.999997064267793,-1.2246432039123E-16));
#6521=DIRECTION('',(0.0034267831331041,-0.707098477694138,0.707106781186541));
#6522=DIRECTION('center_axis',(0.,1.22464679914735E-16,-1.));
#6523=DIRECTION('ref_axis',(0.00242310870467221,-0.999997064267793,-1.2246432039123E-16));
#6524=DIRECTION('center_axis',(0.,-1.22464679914735E-16,1.));
#6525=DIRECTION('ref_axis',(0.00242310870467221,-0.999997064267793,-1.2246432039123E-16));
#6526=DIRECTION('center_axis',(0.,1.22464679914735E-16,-1.));
#6527=DIRECTION('ref_axis',(1.,0.,0.));
#6528=DIRECTION('center_axis',(0.,-1.22464679914735E-16,1.));
#6529=DIRECTION('ref_axis',(1.,0.,0.));
#6530=DIRECTION('center_axis',(0.,1.22464679914735E-16,-1.));
#6531=DIRECTION('ref_axis',(1.,0.,0.));
#6532=DIRECTION('center_axis',(0.121660197152011,0.992571809205225,1.21554988906708E-16));
#6533=DIRECTION('ref_axis',(0.992571809205225,-0.121660197152011,-1.48990771025846E-17));
#6534=DIRECTION('',(0.,1.22464679914735E-16,-1.));
#6535=DIRECTION('',(-0.992571809205225,0.121660197152011,1.48990771025846E-17));
#6536=DIRECTION('',(0.,1.22464679914735E-16,-1.));
#6537=DIRECTION('center_axis',(0.,1.22464679914735E-16,-1.));
#6538=DIRECTION('ref_axis',(3.70074341541624E-15,1.,1.22464679914735E-16));
#6539=DIRECTION('',(0.,1.22464679914735E-16,-1.));
#6540=DIRECTION('center_axis',(0.,-1.22464679914735E-16,1.));
#6541=DIRECTION('ref_axis',(3.70074341541624E-15,1.,1.22464679914735E-16));
#6542=DIRECTION('center_axis',(-7.91304169717665E-19,1.,1.22464679914735E-16));
#6543=DIRECTION('ref_axis',(1.,7.91304169717665E-19,9.69068118596693E-35));
#6544=DIRECTION('',(0.,1.22464679914735E-16,-1.));
#6545=DIRECTION('',(-1.,-7.91304169717665E-19,-9.69068118596693E-35));
#6546=DIRECTION('center_axis',(0.,1.22464679914735E-16,-1.));
#6547=DIRECTION('ref_axis',(-0.111971091458059,0.993711464499475,1.21694556427531E-16));
#6548=DIRECTION('',(0.,1.22464679914735E-16,-1.));
#6549=DIRECTION('center_axis',(0.,-1.22464679914735E-16,1.));
#6550=DIRECTION('ref_axis',(-0.111971091458059,0.993711464499475,1.21694556427531E-16));
#6551=DIRECTION('center_axis',(-0.111971091458068,0.993711464499474,1.21694556427531E-16));
#6552=DIRECTION('ref_axis',(0.993711464499474,0.111971091458068,1.37125038751159E-17));
#6553=DIRECTION('',(0.,1.22464679914735E-16,-1.));
#6554=DIRECTION('',(-0.993711464499474,-0.111971091458068,-1.37125038751159E-17));
#6555=DIRECTION('center_axis',(0.,1.22464679914735E-16,-1.));
#6556=DIRECTION('ref_axis',(-0.705322576499994,0.708886495201743,8.681355773076E-17));
#6557=DIRECTION('',(0.,1.22464679914735E-16,-1.));
#6558=DIRECTION('center_axis',(0.,-1.22464679914735E-16,1.));
#6559=DIRECTION('ref_axis',(-0.705322576499994,0.708886495201743,8.681355773076E-17));
#6560=DIRECTION('center_axis',(-0.705322576499999,0.708886495201738,8.68135577307594E-17));
#6561=DIRECTION('ref_axis',(0.708886495201738,0.705322576499999,8.63771035677088E-17));
#6562=DIRECTION('',(0.,1.22464679914735E-16,-1.));
#6563=DIRECTION('',(-0.708886495201738,-0.705322576499999,-8.63771035677088E-17));
#6564=DIRECTION('center_axis',(0.,1.22464679914735E-16,-1.));
#6565=DIRECTION('ref_axis',(-1.,-1.66533453693774E-15,-2.03944661017034E-31));
#6566=DIRECTION('',(0.,1.22464679914735E-16,-1.));
#6567=DIRECTION('center_axis',(0.,-1.22464679914735E-16,1.));
#6568=DIRECTION('ref_axis',(-1.,-1.66533453693774E-15,-2.03944661017034E-31));
#6569=DIRECTION('center_axis',(-1.,0.,0.));
#6570=DIRECTION('ref_axis',(0.,1.,1.22464679914735E-16));
#6571=DIRECTION('',(0.,1.22464679914735E-16,-1.));
#6572=DIRECTION('',(0.,-1.,-1.22464679914735E-16));
#6573=DIRECTION('center_axis',(0.,1.22464679914735E-16,-1.));
#6574=DIRECTION('ref_axis',(-0.713859961881135,-0.700288479716085,-8.57606045164069E-17));
#6575=DIRECTION('',(0.,1.22464679914735E-16,-1.));
#6576=DIRECTION('center_axis',(0.,-1.22464679914735E-16,1.));
#6577=DIRECTION('ref_axis',(-0.713859961881135,-0.700288479716085,-8.57606045164069E-17));
#6578=DIRECTION('center_axis',(-0.71385996188113,-0.700288479716089,-8.57606045164075E-17));
#6579=DIRECTION('ref_axis',(-0.700288479716089,0.71385996188113,8.74226317357177E-17));
#6580=DIRECTION('',(0.,1.22464679914735E-16,-1.));
#6581=DIRECTION('',(0.700288479716089,-0.71385996188113,-8.74226317357177E-17));
#6582=DIRECTION('center_axis',(0.,1.22464679914735E-16,-1.));
#6583=DIRECTION('ref_axis',(-0.0633304877101173,-0.997992609855604,-1.22218845523238E-16));
#6584=DIRECTION('',(0.,1.22464679914735E-16,-1.));
#6585=DIRECTION('center_axis',(0.,-1.22464679914735E-16,1.));
#6586=DIRECTION('ref_axis',(-0.0633304877101173,-0.997992609855604,-1.22218845523238E-16));
#6587=DIRECTION('center_axis',(-0.063330487710117,-0.997992609855603,-1.22218845523238E-16));
#6588=DIRECTION('ref_axis',(-0.997992609855604,0.063330487710117,7.75574790626356E-18));
#6589=DIRECTION('',(0.,1.22464679914735E-16,-1.));
#6590=DIRECTION('',(0.997992609855604,-0.063330487710117,-7.75574790626356E-18));
#6591=DIRECTION('center_axis',(0.,1.22464679914735E-16,-1.));
#6592=DIRECTION('ref_axis',(-1.18423789293273E-14,-1.,-1.22464679914735E-16));
#6593=DIRECTION('',(0.,1.22464679914735E-16,-1.));
#6594=DIRECTION('center_axis',(0.,-1.22464679914735E-16,1.));
#6595=DIRECTION('ref_axis',(-1.18423789293273E-14,-1.,-1.22464679914735E-16));
#6596=DIRECTION('center_axis',(0.,-1.,-1.22464679914735E-16));
#6597=DIRECTION('ref_axis',(-1.,0.,0.));
#6598=DIRECTION('',(0.,1.22464679914735E-16,-1.));
#6599=DIRECTION('',(1.,0.,0.));
#6600=DIRECTION('center_axis',(0.,1.22464679914735E-16,-1.));
#6601=DIRECTION('ref_axis',(0.00242310870467221,-0.999997064267793,-1.2246432039123E-16));
#6602=DIRECTION('',(0.,-1.22464679914735E-16,1.));
#6603=DIRECTION('center_axis',(0.,-1.22464679914735E-16,1.));
#6604=DIRECTION('ref_axis',(0.00242310870467221,-0.999997064267793,-1.2246432039123E-16));
#6605=DIRECTION('center_axis',(0.,1.22464679914735E-16,-1.));
#6606=DIRECTION('ref_axis',(1.,0.,0.));
#6607=DIRECTION('',(0.,1.22464679914735E-16,-1.));
#6608=DIRECTION('center_axis',(0.,1.22464679914735E-16,-1.));
#6609=DIRECTION('ref_axis',(1.,0.,0.));
#6610=DIRECTION('center_axis',(0.,-1.22464679914735E-16,1.));
#6611=DIRECTION('ref_axis',(-2.22044604925031E-16,1.,1.22464679914735E-16));
#6612=DIRECTION('',(0.,1.22464679914735E-16,-1.));
#6613=DIRECTION('center_axis',(0.,1.22464679914735E-16,-1.));
#6614=DIRECTION('ref_axis',(-2.22044604925031E-16,1.,1.22464679914735E-16));
#6615=DIRECTION('center_axis',(0.,1.22464679914735E-16,-1.));
#6616=DIRECTION('ref_axis',(1.,0.,0.));
#6617=DIRECTION('center_axis',(0.,1.22464679914735E-16,-1.));
#6618=DIRECTION('ref_axis',(-2.22044604925031E-16,1.,1.22464679914735E-16));
#6619=DIRECTION('center_axis',(0.,1.22464679914735E-16,-1.));
#6620=DIRECTION('ref_axis',(1.,0.,0.));
#6621=DIRECTION('center_axis',(0.,1.22464679914735E-16,-1.));
#6622=DIRECTION('ref_axis',(-2.22044604925031E-16,1.,1.22464679914735E-16));
#6623=DIRECTION('center_axis',(0.,-1.22464679914735E-16,1.));
#6624=DIRECTION('ref_axis',(1.,0.,0.));
#6625=DIRECTION('center_axis',(0.,1.22464679914735E-16,-1.));
#6626=DIRECTION('ref_axis',(1.,0.,0.));
#6627=DIRECTION('center_axis',(0.,-1.22464679914735E-16,1.));
#6628=DIRECTION('ref_axis',(1.,0.,0.));
#6629=DIRECTION('center_axis',(0.,-1.22464679914735E-16,1.));
#6630=DIRECTION('ref_axis',(1.,0.,0.));
#6631=DIRECTION('',(0.00342678313310414,-0.707098477694131,-0.707106781186548));
#6632=DIRECTION('center_axis',(0.,1.22464679914735E-16,-1.));
#6633=DIRECTION('ref_axis',(0.00242310870467221,-0.999997064267793,-1.2246432039123E-16));
#6634=DIRECTION('',(0.,-0.707106781186554,-0.707106781186541));
#6635=DIRECTION('center_axis',(0.,1.22464679914735E-16,-1.));
#6636=DIRECTION('ref_axis',(0.00242310870467221,-0.999997064267793,-1.2246432039123E-16));
#6637=DIRECTION('center_axis',(0.,-0.707106781186547,0.707106781186548));
#6638=DIRECTION('ref_axis',(-1.,0.,0.));
#6639=DIRECTION('',(0.,-0.707106781186548,-0.707106781186547));
#6640=DIRECTION('',(-1.,0.,0.));
#6641=DIRECTION('center_axis',(0.,1.22464679914735E-16,-1.));
#6642=DIRECTION('ref_axis',(-1.18423789293273E-14,-1.,-1.22464679914735E-16));
#6643=DIRECTION('',(-0.0447814173156507,-0.70568734200296,-0.707106781186546));
#6644=DIRECTION('center_axis',(0.,1.22464679914735E-16,-1.));
#6645=DIRECTION('ref_axis',(-1.18423789293273E-14,-1.,-1.22464679914735E-16));
#6646=DIRECTION('center_axis',(-0.044781417315675,-0.705687342002957,0.707106781186548));
#6647=DIRECTION('ref_axis',(-0.998000636867369,7.74024134983378E-18,-0.0632038670678177));
#6648=DIRECTION('',(-0.997992609855604,0.063330487710117,7.75574790626356E-18));
#6649=DIRECTION('',(-0.0447814173156758,-0.705687342002958,-0.707106781186547));
#6650=DIRECTION('center_axis',(0.,1.22464679914735E-16,-1.));
#6651=DIRECTION('ref_axis',(-0.0633304877101173,-0.997992609855603,-1.22218845523238E-16));
#6652=DIRECTION('',(-0.504775219863726,-0.495178732794059,-0.707106781186545));
#6653=DIRECTION('center_axis',(0.,1.22464679914735E-16,-1.));
#6654=DIRECTION('ref_axis',(-0.0633304877101173,-0.997992609855603,-1.22218845523238E-16));
#6655=DIRECTION('center_axis',(-0.504775219863718,-0.495178732794066,0.707106781186546));
#6656=DIRECTION('ref_axis',(-0.813897332858798,7.11530468011978E-17,-0.581008719009737));
#6657=DIRECTION('',(-0.700288479716089,0.71385996188113,8.74226317357177E-17));
#6658=DIRECTION('',(-0.504775219863717,-0.495178732794063,-0.707106781186549));
#6659=DIRECTION('center_axis',(0.,1.22464679914735E-16,-1.));
#6660=DIRECTION('ref_axis',(-0.713859961881135,-0.700288479716084,-8.57606045164069E-17));
#6661=DIRECTION('',(-0.707106781186546,-4.62368177042778E-15,-0.707106781186549));
#6662=DIRECTION('center_axis',(0.,1.22464679914735E-16,-1.));
#6663=DIRECTION('ref_axis',(-0.713859961881135,-0.700288479716085,-8.57606045164069E-17));
#6664=DIRECTION('center_axis',(-0.707106781186549,-8.65956056235492E-17,
0.707106781186546));
#6665=DIRECTION('ref_axis',(-0.707106781186546,8.65956056235495E-17,-0.707106781186549));
#6666=DIRECTION('',(0.,1.,1.22464679914735E-16));
#6667=DIRECTION('',(-0.707106781186546,8.65956056235495E-17,-0.707106781186549));
#6668=DIRECTION('center_axis',(0.,1.22464679914735E-16,-1.));
#6669=DIRECTION('ref_axis',(-1.,-1.66533453693774E-15,-2.03944661017034E-31));
#6670=DIRECTION('',(-0.498738376767117,0.501258447848715,-0.707106781186546));
#6671=DIRECTION('center_axis',(0.,1.22464679914735E-16,-1.));
#6672=DIRECTION('ref_axis',(-1.,-1.66533453693774E-15,-2.03944661017034E-31));
#6673=DIRECTION('center_axis',(-0.498738376767116,0.501258447848713,0.707106781186548));
#6674=DIRECTION('ref_axis',(-0.817183320658714,7.05859283223419E-17,-0.576377845199828));
#6675=DIRECTION('',(0.708886495201738,0.705322576499999,8.63771035677088E-17));
#6676=DIRECTION('',(-0.498738376767118,0.501258447848713,-0.707106781186547));
#6677=DIRECTION('center_axis',(0.,1.22464679914735E-16,-1.));
#6678=DIRECTION('ref_axis',(-0.705322576499994,0.708886495201743,8.681355773076E-17));
#6679=DIRECTION('',(-0.0791755180668617,0.702660115090393,-0.707106781186547));
#6680=DIRECTION('center_axis',(0.,1.22464679914735E-16,-1.));
#6681=DIRECTION('ref_axis',(-0.705322576499994,0.708886495201743,8.681355773076E-17));
#6682=DIRECTION('center_axis',(-0.0791755180668589,0.702660115090392,0.707106781186549));
#6683=DIRECTION('ref_axis',(-0.993789574232718,1.36273433877158E-17,-0.111275703306486));
#6684=DIRECTION('',(0.993711464499474,0.111971091458068,1.37125038751159E-17));
#6685=DIRECTION('',(-0.0791755180668616,0.702660115090394,-0.707106781186547));
#6686=DIRECTION('center_axis',(0.,1.22464679914735E-16,-1.));
#6687=DIRECTION('ref_axis',(-0.111971091458059,0.993711464499475,1.21694556427531E-16));
#6688=DIRECTION('',(-1.25607396694702E-14,0.707106781186547,-0.707106781186548));
#6689=DIRECTION('center_axis',(0.,1.22464679914735E-16,-1.));
#6690=DIRECTION('ref_axis',(-0.111971091458059,0.993711464499475,1.21694556427531E-16));
#6691=DIRECTION('center_axis',(-5.59536544388551E-19,0.707106781186547,
0.707106781186548));
#6692=DIRECTION('ref_axis',(-1.,9.69068118596692E-35,-7.91304169717664E-19));
#6693=DIRECTION('',(0.,0.707106781186548,-0.707106781186547));
#6694=DIRECTION('',(1.,7.91304169717665E-19,9.69068118596693E-35));
#6695=DIRECTION('center_axis',(0.,1.22464679914735E-16,-1.));
#6696=DIRECTION('ref_axis',(3.70074341541624E-15,1.,1.22464679914735E-16));
#6697=DIRECTION('',(0.086026750406675,0.701854257103615,-0.707106781186548));
#6698=DIRECTION('center_axis',(0.,1.22464679914735E-16,-1.));
#6699=DIRECTION('ref_axis',(3.70074341541624E-15,1.,1.22464679914735E-16));
#6700=DIRECTION('center_axis',(0.086026750406679,0.701854257103615,0.707106781186547));
#6701=DIRECTION('ref_axis',(-0.992680551218392,-1.4790024070839E-17,0.120769711570196));
#6702=DIRECTION('',(0.0860267504066797,0.701854257103614,-0.707106781186548));
#6703=DIRECTION('',(0.992571809205225,-0.121660197152011,-1.48990771025846E-17));
#6704=DIRECTION('center_axis',(0.,1.22464679914735E-16,-1.));
#6705=DIRECTION('ref_axis',(0.12166019715201,0.992571809205225,1.21554988906708E-16));
#6706=DIRECTION('',(0.701854257103614,0.0860267504066782,-0.707106781186548));
#6707=DIRECTION('center_axis',(0.,-1.22464679914735E-16,1.));
#6708=DIRECTION('ref_axis',(0.12166019715201,0.992571809205225,1.21554988906708E-16));
#6709=DIRECTION('center_axis',(0.,1.22464679914735E-16,-1.));
#6710=DIRECTION('ref_axis',(0.12166019715201,0.992571809205225,1.21554988906708E-16));
#6711=DIRECTION('center_axis',(0.701854257103616,0.0860267504066792,0.707106781186546));
#6712=DIRECTION('ref_axis',(-0.709737901988186,-8.62721828028442E-17,0.704465833437937));
#6713=DIRECTION('',(0.121660197152011,-0.992571809205225,-1.21554988906708E-16));
#6714=DIRECTION('',(0.701854257103613,0.0860267504066799,-0.707106781186549));
#6715=DIRECTION('',(-0.121660197152011,0.992571809205225,1.21554988906708E-16));
#6716=DIRECTION('center_axis',(0.,1.22464679914735E-16,-1.));
#6717=DIRECTION('ref_axis',(1.,3.92278802034127E-15,4.80402979284452E-31));
#6718=DIRECTION('center_axis',(0.,1.22464679914735E-16,-1.));
#6719=DIRECTION('ref_axis',(1.,3.92278802034127E-15,4.80402979284452E-31));
#6720=DIRECTION('',(0.707106781186547,1.65668806430733E-15,-0.707106781186548));
#6721=DIRECTION('center_axis',(0.,-1.22464679914735E-16,1.));
#6722=DIRECTION('ref_axis',(1.,3.92278802034127E-15,4.80402979284452E-31));
#6723=DIRECTION('center_axis',(0.707106781186548,6.98541037004396E-17,0.707106781186547));
#6724=DIRECTION('ref_axis',(-0.707106781186547,-8.65956056235493E-17,0.707106781186548));
#6725=DIRECTION('',(2.21253300755314E-16,-1.,-1.22464679914735E-16));
#6726=DIRECTION('',(0.707106781186547,8.65956056235493E-17,-0.707106781186548));
#6727=DIRECTION('',(-2.21253300755314E-16,1.,1.22464679914735E-16));
#6728=DIRECTION('center_axis',(0.,1.22464679914735E-16,-1.));
#6729=DIRECTION('ref_axis',(0.993711464499475,-0.111971091458059,-1.37125038751148E-17));
#6730=DIRECTION('center_axis',(0.,1.22464679914735E-16,-1.));
#6731=DIRECTION('ref_axis',(0.993711464499475,-0.111971091458059,-1.37125038751148E-17));
#6732=DIRECTION('',(0.702660115090394,-0.0791755180668553,-0.707106781186547));
#6733=DIRECTION('center_axis',(0.,-1.22464679914735E-16,1.));
#6734=DIRECTION('ref_axis',(0.993711464499475,-0.111971091458059,-1.37125038751148E-17));
#6735=DIRECTION('center_axis',(0.702660115090393,-0.0791755180668589,0.707106781186548));
#6736=DIRECTION('ref_axis',(-0.709333598508652,-8.63220376296546E-17,0.704872928992714));
#6737=DIRECTION('',(0.702660115090394,-0.0791755180668553,-0.707106781186547));
#6738=DIRECTION('',(0.111971091458068,0.993711464499474,1.21694556427531E-16));
#6739=DIRECTION('',(-0.111971091458068,-0.993711464499474,-1.21694556427531E-16));
#6740=DIRECTION('center_axis',(0.,1.22464679914735E-16,-1.));
#6741=DIRECTION('ref_axis',(0.708886495201743,-0.705322576499993,-8.63771035677081E-17));
#6742=DIRECTION('center_axis',(0.,1.22464679914735E-16,-1.));
#6743=DIRECTION('ref_axis',(0.708886495201743,-0.705322576499994,-8.63771035677081E-17));
#6744=DIRECTION('',(0.501258447848718,-0.498738376767112,-0.707106781186548));
#6745=DIRECTION('center_axis',(0.,-1.22464679914735E-16,1.));
#6746=DIRECTION('ref_axis',(0.708886495201743,-0.705322576499994,-8.63771035677081E-17));
#6747=DIRECTION('center_axis',(0.501258447848716,-0.498738376767119,0.707106781186545));
#6748=DIRECTION('ref_axis',(-0.815811569646784,-7.08235047989531E-17,0.578317804351942));
#6749=DIRECTION('',(0.501258447848714,-0.498738376767113,-0.70710678118655));
#6750=DIRECTION('',(0.705322576499999,0.708886495201738,8.68135577307594E-17));
#6751=DIRECTION('',(-0.705322576499999,-0.708886495201738,-8.68135577307594E-17));
#6752=DIRECTION('center_axis',(0.,1.22464679914735E-16,-1.));
#6753=DIRECTION('ref_axis',(-1.44328993201271E-15,-1.,-1.22464679914735E-16));
#6754=DIRECTION('center_axis',(0.,1.22464679914735E-16,-1.));
#6755=DIRECTION('ref_axis',(-1.44328993201271E-15,-1.,-1.22464679914735E-16));
#6756=DIRECTION('',(-7.85046229341885E-16,-0.707106781186549,-0.707106781186546));
#6757=DIRECTION('center_axis',(0.,-1.22464679914735E-16,1.));
#6758=DIRECTION('ref_axis',(-1.44328993201271E-15,-1.,-1.22464679914735E-16));
#6759=DIRECTION('center_axis',(1.57009245868378E-16,-0.707106781186549,
0.707106781186546));
#6760=DIRECTION('ref_axis',(-1.,-2.71926214689379E-32,2.22044604925032E-16));
#6761=DIRECTION('',(0.,-0.707106781186546,-0.707106781186549));
#6762=DIRECTION('',(1.,2.22044604925031E-16,2.71926214689378E-32));
#6763=DIRECTION('',(-1.,-2.22044604925031E-16,-2.71926214689378E-32));
#6764=DIRECTION('center_axis',(0.,1.22464679914735E-16,-1.));
#6765=DIRECTION('ref_axis',(-0.700288479716085,-0.713859961881135,-8.74226317357183E-17));
#6766=DIRECTION('center_axis',(0.,1.22464679914735E-16,-1.));
#6767=DIRECTION('ref_axis',(-0.700288479716085,-0.713859961881135,-8.74226317357183E-17));
#6768=DIRECTION('',(-0.495178732794061,-0.504775219863721,-0.707106781186547));
#6769=DIRECTION('center_axis',(0.,-1.22464679914735E-16,1.));
#6770=DIRECTION('ref_axis',(-0.700288479716085,-0.713859961881135,-8.74226317357183E-17));
#6771=DIRECTION('center_axis',(-0.495178732794066,-0.504775219863719,0.707106781186546));
#6772=DIRECTION('ref_axis',(-0.819120891857569,7.02483028577242E-17,-0.573620924062626));
#6773=DIRECTION('',(-0.495178732794064,-0.504775219863716,-0.707106781186549));
#6774=DIRECTION('',(0.71385996188113,-0.700288479716089,-8.57606045164075E-17));
#6775=DIRECTION('',(-0.71385996188113,0.700288479716089,8.57606045164075E-17));
#6776=DIRECTION('center_axis',(0.,1.22464679914735E-16,-1.));
#6777=DIRECTION('ref_axis',(-0.997992609855603,-0.0633304877101176,-7.75574790626363E-18));
#6778=DIRECTION('center_axis',(0.,1.22464679914735E-16,-1.));
#6779=DIRECTION('ref_axis',(-0.997992609855603,-0.0633304877101176,-7.75574790626363E-18));
#6780=DIRECTION('',(-0.705687342002959,-0.0447814173156757,-0.707106781186546));
#6781=DIRECTION('center_axis',(0.,-1.22464679914735E-16,1.));
#6782=DIRECTION('ref_axis',(-0.997992609855603,-0.0633304877101176,-7.75574790626363E-18));
#6783=DIRECTION('center_axis',(-0.705687342002957,-0.0447814173156752,0.707106781186548));
#6784=DIRECTION('ref_axis',(-0.707816856590717,8.65085590544045E-17,-0.706395992008758));
#6785=DIRECTION('',(-0.705687342002958,-0.0447814173156758,-0.707106781186547));
#6786=DIRECTION('',(0.0633304877101172,-0.997992609855604,-1.22218845523238E-16));
#6787=DIRECTION('',(-0.0633304877101172,0.997992609855604,1.22218845523238E-16));
#6788=DIRECTION('center_axis',(0.,1.22464679914735E-16,-1.));
#6789=DIRECTION('ref_axis',(-1.,-1.20644235342523E-14,-1.47746576647801E-30));
#6790=DIRECTION('center_axis',(0.,1.22464679914735E-16,-1.));
#6791=DIRECTION('ref_axis',(-1.,-1.20644235342523E-14,-1.47746576647801E-30));
#6792=DIRECTION('',(-0.707106781186549,-6.19377422911154E-15,-0.707106781186546));
#6793=DIRECTION('center_axis',(0.,-1.22464679914735E-16,1.));
#6794=DIRECTION('ref_axis',(-1.,-1.20644235342523E-14,-1.47746576647801E-30));
#6795=DIRECTION('center_axis',(-0.707106781186547,-2.43604851491927E-16,
0.707106781186548));
#6796=DIRECTION('ref_axis',(-0.707106781186548,8.65956056235493E-17,-0.707106781186547));
#6797=DIRECTION('',(-2.22044604925031E-16,1.,1.22464679914735E-16));
#6798=DIRECTION('',(-0.707106781186544,8.65956056235498E-17,-0.707106781186551));
#6799=DIRECTION('',(2.22044604925031E-16,-1.,-1.22464679914735E-16));
#6800=DIRECTION('center_axis',(0.,1.22464679914735E-16,-1.));
#6801=DIRECTION('ref_axis',(-0.999997064267793,0.00242310870464513,2.96745231912974E-19));
#6802=DIRECTION('',(-0.707098477694137,0.00342678313306651,-0.707106781186542));
#6803=DIRECTION('center_axis',(0.,-1.22464679914735E-16,1.));
#6804=DIRECTION('ref_axis',(-0.999997064267793,0.00242310870464512,2.96745231912974E-19));
#6805=DIRECTION('center_axis',(0.,1.22464679914735E-16,-1.));
#6806=DIRECTION('ref_axis',(-0.999997064267794,0.00242310870464513,2.96745231912974E-19));
#6807=DIRECTION('center_axis',(0.,-1.22464679914735E-16,1.));
#6808=DIRECTION('ref_axis',(-2.22044604925031E-16,1.,1.22464679914735E-16));
#6809=DIRECTION('center_axis',(0.,-1.22464679914735E-16,1.));
#6810=DIRECTION('ref_axis',(-2.22044604925031E-16,1.,1.22464679914735E-16));
#6811=DIRECTION('center_axis',(-0.992571809205225,-0.121660197152011,-1.48990771025846E-17));
#6812=DIRECTION('ref_axis',(-0.121660197152011,0.992571809205225,1.21554988906708E-16));
#6813=DIRECTION('',(0.,1.22464679914735E-16,-1.));
#6814=DIRECTION('',(0.,1.22464679914735E-16,-1.));
#6815=DIRECTION('center_axis',(0.,-1.22464679914735E-16,1.));
#6816=DIRECTION('ref_axis',(1.,3.92278802034127E-15,4.80402979284452E-31));
#6817=DIRECTION('',(0.,1.22464679914735E-16,-1.));
#6818=DIRECTION('center_axis',(-1.,-2.21253300755314E-16,-2.70957146570782E-32));
#6819=DIRECTION('ref_axis',(-2.21253300755314E-16,1.,1.22464679914735E-16));
#6820=DIRECTION('',(0.,1.22464679914735E-16,-1.));
#6821=DIRECTION('center_axis',(0.,-1.22464679914735E-16,1.));
#6822=DIRECTION('ref_axis',(0.993711464499475,-0.111971091458059,-1.37125038751148E-17));
#6823=DIRECTION('',(0.,1.22464679914735E-16,-1.));
#6824=DIRECTION('center_axis',(-0.993711464499474,0.111971091458068,1.37125038751158E-17));
#6825=DIRECTION('ref_axis',(0.111971091458068,0.993711464499474,1.21694556427531E-16));
#6826=DIRECTION('',(0.,1.22464679914735E-16,-1.));
#6827=DIRECTION('center_axis',(0.,-1.22464679914735E-16,1.));
#6828=DIRECTION('ref_axis',(0.708886495201743,-0.705322576499994,-8.63771035677081E-17));
#6829=DIRECTION('',(0.,1.22464679914735E-16,-1.));
#6830=DIRECTION('center_axis',(-0.708886495201738,0.705322576499999,8.63771035677088E-17));
#6831=DIRECTION('ref_axis',(0.705322576499999,0.708886495201738,8.68135577307594E-17));
#6832=DIRECTION('',(0.,1.22464679914735E-16,-1.));
#6833=DIRECTION('center_axis',(0.,-1.22464679914735E-16,1.));
#6834=DIRECTION('ref_axis',(-1.44328993201271E-15,-1.,-1.22464679914735E-16));
#6835=DIRECTION('',(0.,1.22464679914735E-16,-1.));
#6836=DIRECTION('center_axis',(-2.22044604925031E-16,1.,1.22464679914735E-16));
#6837=DIRECTION('ref_axis',(1.,2.22044604925031E-16,2.71926214689378E-32));
#6838=DIRECTION('',(0.,1.22464679914735E-16,-1.));
#6839=DIRECTION('center_axis',(0.,-1.22464679914735E-16,1.));
#6840=DIRECTION('ref_axis',(-0.700288479716085,-0.713859961881135,-8.74226317357183E-17));
#6841=DIRECTION('',(0.,1.22464679914735E-16,-1.));
#6842=DIRECTION('center_axis',(0.700288479716089,0.71385996188113,8.74226317357178E-17));
#6843=DIRECTION('ref_axis',(0.71385996188113,-0.700288479716089,-8.57606045164075E-17));
#6844=DIRECTION('',(0.,1.22464679914735E-16,-1.));
#6845=DIRECTION('center_axis',(0.,-1.22464679914735E-16,1.));
#6846=DIRECTION('ref_axis',(-0.997992609855604,-0.0633304877101176,-7.75574790626363E-18));
#6847=DIRECTION('',(0.,1.22464679914735E-16,-1.));
#6848=DIRECTION('center_axis',(0.997992609855603,0.0633304877101172,7.75574790626358E-18));
#6849=DIRECTION('ref_axis',(0.0633304877101172,-0.997992609855604,-1.22218845523238E-16));
#6850=DIRECTION('',(0.,1.22464679914735E-16,-1.));
#6851=DIRECTION('center_axis',(0.,-1.22464679914735E-16,1.));
#6852=DIRECTION('ref_axis',(-1.,-1.20644235342523E-14,-1.47746576647801E-30));
#6853=DIRECTION('',(0.,1.22464679914735E-16,-1.));
#6854=DIRECTION('center_axis',(1.,2.22044604925031E-16,2.71926214689378E-32));
#6855=DIRECTION('ref_axis',(2.22044604925031E-16,-1.,-1.22464679914735E-16));
#6856=DIRECTION('',(0.,-1.22464679914735E-16,1.));
#6857=DIRECTION('center_axis',(0.,1.22464679914735E-16,-1.));
#6858=DIRECTION('ref_axis',(-0.999997064267793,0.00242310870464513,2.96745231912974E-19));
#6859=DIRECTION('center_axis',(0.,1.22464679914735E-16,-1.));
#6860=DIRECTION('ref_axis',(1.,0.,0.));
#6861=DIRECTION('center_axis',(0.,-1.22464679914735E-16,1.));
#6862=DIRECTION('ref_axis',(1.,0.,0.));
#6863=DIRECTION('center_axis',(0.,1.22464679914735E-16,-1.));
#6864=DIRECTION('ref_axis',(-2.22044604925031E-16,1.,1.22464679914735E-16));
#6865=DIRECTION('center_axis',(0.,-1.22464679914735E-16,1.));
#6866=DIRECTION('ref_axis',(-2.22044604925031E-16,1.,1.22464679914735E-16));
#6867=DIRECTION('center_axis',(0.,-1.22464679914735E-16,1.));
#6868=DIRECTION('ref_axis',(1.,0.,0.));
#6869=DIRECTION('center_axis',(-8.16185220949039E-33,-9.18840920464028E-33,
1.));
#6870=DIRECTION('ref_axis',(-2.22044604925031E-16,1.,1.22464679914735E-16));
#6871=DIRECTION('center_axis',(0.,-1.22464679914735E-16,1.));
#6872=DIRECTION('ref_axis',(1.,0.,0.));
#6873=DIRECTION('center_axis',(0.,-1.22464679914735E-16,1.));
#6874=DIRECTION('ref_axis',(1.,0.,0.));
#6875=DIRECTION('center_axis',(0.,-1.22464679914735E-16,1.));
#6876=DIRECTION('ref_axis',(1.,0.,0.));
#6877=DIRECTION('center_axis',(3.24468512908471E-49,-3.01569151445155E-49,
1.));
#6878=DIRECTION('ref_axis',(1.,0.,0.));
#6879=DIRECTION('center_axis',(0.,1.22464679914735E-16,-1.));
#6880=DIRECTION('ref_axis',(-2.22044604925031E-16,1.,1.22464679914735E-16));
#6881=DIRECTION('center_axis',(0.,-1.22464679914735E-16,1.));
#6882=DIRECTION('ref_axis',(-2.22044604925031E-16,1.,1.22464679914735E-16));
#6883=DIRECTION('',(2.43604851491926E-16,-0.707106781186546,-0.707106781186549));
#6884=DIRECTION('center_axis',(0.,-1.22464679914735E-16,1.));
#6885=DIRECTION('ref_axis',(-2.22044604925031E-16,1.,1.22464679914735E-16));
#6886=DIRECTION('',(0.,-1.22464679914735E-16,1.));
#6887=DIRECTION('center_axis',(0.,1.22464679914735E-16,-1.));
#6888=DIRECTION('ref_axis',(1.,0.,0.));
#6889=DIRECTION('center_axis',(0.,-1.22464679914735E-16,1.));
#6890=DIRECTION('ref_axis',(1.,0.,0.));
#6891=DIRECTION('',(-0.707106781186548,-1.80858895911741E-32,-0.707106781186548));
#6892=DIRECTION('center_axis',(0.,1.22464679914735E-16,-1.));
#6893=DIRECTION('ref_axis',(1.,0.,0.));
#6894=DIRECTION('',(0.,-1.22464679914735E-16,1.));
#6895=DIRECTION('center_axis',(0.,1.22464679914735E-16,-1.));
#6896=DIRECTION('ref_axis',(1.,0.,0.));
#6897=DIRECTION('',(0.707106781186546,-1.73191211247099E-16,0.707106781186549));
#6898=DIRECTION('center_axis',(0.,-1.22464679914735E-16,1.));
#6899=DIRECTION('ref_axis',(1.,0.,0.));
#6900=DIRECTION('center_axis',(0.,1.22464679914735E-16,-1.));
#6901=DIRECTION('ref_axis',(1.,0.,0.));
#6902=DIRECTION('',(0.,-1.22464679914735E-16,1.));
#6903=DIRECTION('center_axis',(0.,-1.22464679914735E-16,1.));
#6904=DIRECTION('ref_axis',(-2.22044604925031E-16,1.,1.22464679914735E-16));
#6905=DIRECTION('',(0.,-1.22464679914735E-16,1.));
#6906=DIRECTION('center_axis',(0.,1.22464679914735E-16,-1.));
#6907=DIRECTION('ref_axis',(1.,0.,0.));
#6908=DIRECTION('',(0.,-1.22464679914735E-16,1.));
#6909=DIRECTION('center_axis',(0.,1.22464679914735E-16,-1.));
#6910=DIRECTION('ref_axis',(0.12166019715201,0.992571809205225,1.21554988906708E-16));
#6911=DIRECTION('axis',(0.,0.,1.));
#6912=DIRECTION('refdir',(1.,0.,0.));
#6913=DIRECTION('center_axis',(-1.,0.,0.));
#6914=DIRECTION('ref_axis',(0.,-1.,-1.22464679914735E-16));
#6915=DIRECTION('center_axis',(-1.,0.,0.));
#6916=DIRECTION('ref_axis',(0.,-1.,-1.22464679914735E-16));
#6917=DIRECTION('',(-0.707106781186545,0.707106781186549,1.73191211247099E-16));
#6918=DIRECTION('center_axis',(1.,0.,0.));
#6919=DIRECTION('ref_axis',(0.,-1.,-1.22464679914735E-16));
#6920=DIRECTION('center_axis',(1.,0.,0.));
#6921=DIRECTION('ref_axis',(0.,-1.,-1.22464679914735E-16));
#6922=DIRECTION('',(-1.,0.,0.));
#6923=DIRECTION('center_axis',(-1.,0.,0.));
#6924=DIRECTION('ref_axis',(0.,-1.,-1.22464679914735E-16));
#6925=DIRECTION('center_axis',(1.,0.,0.));
#6926=DIRECTION('ref_axis',(0.,-1.22464679914735E-16,1.));
#6927=DIRECTION('center_axis',(1.,0.,0.));
#6928=DIRECTION('ref_axis',(0.,-1.,-1.22464679914735E-16));
#6929=DIRECTION('',(-0.707106781186548,-0.707106781186548,-1.73191211247099E-16));
#6930=DIRECTION('center_axis',(1.,0.,0.));
#6931=DIRECTION('ref_axis',(0.,-1.,-1.22464679914735E-16));
#6932=DIRECTION('center_axis',(1.,0.,0.));
#6933=DIRECTION('ref_axis',(0.,-1.22464679914735E-16,1.));
#6934=DIRECTION('axis',(0.,0.,1.));
#6935=DIRECTION('refdir',(1.,0.,0.));
#6936=DIRECTION('center_axis',(-1.,0.,0.));
#6937=DIRECTION('ref_axis',(0.,0.,-1.));
#6938=DIRECTION('center_axis',(0.,1.,0.));
#6939=DIRECTION('ref_axis',(0.,0.,1.));
#6940=DIRECTION('center_axis',(1.,0.,0.));
#6941=DIRECTION('ref_axis',(0.,0.,-1.));
#6942=DIRECTION('center_axis',(0.,1.,1.22464679914735E-16));
#6943=DIRECTION('ref_axis',(1.,0.,0.));
#6944=DIRECTION('center_axis',(1.22464679914735E-15,-1.,-1.22464679914735E-16));
#6945=DIRECTION('ref_axis',(1.,1.22464679914735E-15,1.49975978266186E-31));
#6946=DIRECTION('center_axis',(1.22464679914735E-15,-1.,-1.22464679914735E-16));
#6947=DIRECTION('ref_axis',(0.,1.22464679914735E-16,-1.));
#6948=DIRECTION('axis',(0.,0.,1.));
#6949=DIRECTION('refdir',(1.,0.,0.));
#6950=DIRECTION('center_axis',(0.,0.,-1.));
#6951=DIRECTION('ref_axis',(1.,0.,0.));
#6952=DIRECTION('center_axis',(0.,-1.22464679914735E-16,1.));
#6953=DIRECTION('ref_axis',(0.,-1.,-1.22464679914735E-16));
#6954=DIRECTION('center_axis',(0.,1.,1.22464679914735E-16));
#6955=DIRECTION('ref_axis',(-1.,0.,0.));
#6956=DIRECTION('center_axis',(0.,1.22464679914735E-16,-1.));
#6957=DIRECTION('ref_axis',(1.,0.,0.));
#6958=DIRECTION('center_axis',(0.,-1.22464679914735E-16,1.));
#6959=DIRECTION('ref_axis',(1.,0.,0.));
#6960=DIRECTION('center_axis',(0.,1.,1.22464679914735E-16));
#6961=DIRECTION('ref_axis',(-1.,0.,0.));
#6962=DIRECTION('center_axis',(0.,1.22464679914735E-16,-1.));
#6963=DIRECTION('ref_axis',(1.,0.,0.));
#6964=DIRECTION('center_axis',(0.,1.22464679914735E-16,-1.));
#6965=DIRECTION('ref_axis',(1.,0.,0.));
#6966=DIRECTION('',(0.,-1.22464679914735E-16,1.));
#6967=DIRECTION('center_axis',(0.,-1.22464679914735E-16,1.));
#6968=DIRECTION('ref_axis',(1.,0.,0.));
#6969=DIRECTION('center_axis',(0.,-1.22464679914735E-16,1.));
#6970=DIRECTION('ref_axis',(1.,0.,0.));
#6971=DIRECTION('center_axis',(-0.5,-0.866025403784439,-1.06057523872491E-16));
#6972=DIRECTION('ref_axis',(-0.866025403784439,0.5,6.12323399573677E-17));
#6973=DIRECTION('',(-0.866025403784439,0.5,6.12323399573677E-17));
#6974=DIRECTION('',(0.,1.22464679914735E-16,-1.));
#6975=DIRECTION('',(-0.866025403784439,0.5,6.12323399573677E-17));
#6976=DIRECTION('',(0.,1.22464679914735E-16,-1.));
#6977=DIRECTION('center_axis',(0.5,-0.866025403784439,-1.06057523872491E-16));
#6978=DIRECTION('ref_axis',(-0.866025403784439,-0.5,-6.12323399573677E-17));
#6979=DIRECTION('',(-0.866025403784439,-0.5,-6.12323399573677E-17));
#6980=DIRECTION('',(0.,1.22464679914735E-16,-1.));
#6981=DIRECTION('',(-0.866025403784439,-0.5,-6.12323399573677E-17));
#6982=DIRECTION('center_axis',(1.,0.,0.));
#6983=DIRECTION('ref_axis',(0.,-1.,-1.22464679914735E-16));
#6984=DIRECTION('',(0.,-1.,-1.22464679914735E-16));
#6985=DIRECTION('',(0.,1.22464679914735E-16,-1.));
#6986=DIRECTION('',(0.,-1.,-1.22464679914735E-16));
#6987=DIRECTION('center_axis',(0.5,0.866025403784439,1.06057523872491E-16));
#6988=DIRECTION('ref_axis',(0.866025403784439,-0.5,-6.12323399573677E-17));
#6989=DIRECTION('',(0.866025403784439,-0.5,-6.12323399573677E-17));
#6990=DIRECTION('',(0.,1.22464679914735E-16,-1.));
#6991=DIRECTION('',(0.866025403784439,-0.5,-6.12323399573677E-17));
#6992=DIRECTION('center_axis',(-0.5,0.866025403784439,1.06057523872491E-16));
#6993=DIRECTION('ref_axis',(0.866025403784439,0.5,6.12323399573676E-17));
#6994=DIRECTION('',(0.866025403784439,0.5,6.12323399573676E-17));
#6995=DIRECTION('',(0.,1.22464679914735E-16,-1.));
#6996=DIRECTION('',(0.866025403784439,0.5,6.12323399573676E-17));
#6997=DIRECTION('center_axis',(-1.,6.40987562127855E-16,7.84983366253143E-32));
#6998=DIRECTION('ref_axis',(6.40987562127855E-16,1.,1.22464679914735E-16));
#6999=DIRECTION('',(6.40987562127855E-16,1.,1.22464679914735E-16));
#7000=DIRECTION('',(6.40987562127855E-16,1.,1.22464679914735E-16));
#7001=DIRECTION('center_axis',(0.,1.22464679914735E-16,-1.));
#7002=DIRECTION('ref_axis',(1.,0.,0.));
#7003=DIRECTION('center_axis',(0.,1.22464679914735E-16,-1.));
#7004=DIRECTION('ref_axis',(1.,0.,0.));
#7005=DIRECTION('center_axis',(0.,1.22464679914735E-16,-1.));
#7006=DIRECTION('ref_axis',(1.,0.,0.));
#7007=DIRECTION('',(-0.707106781186547,2.11959791839945E-32,-0.707106781186548));
#7008=DIRECTION('center_axis',(0.,-1.22464679914735E-16,1.));
#7009=DIRECTION('ref_axis',(1.,0.,0.));
#7010=DIRECTION('axis',(0.,0.,1.));
#7011=DIRECTION('refdir',(1.,0.,0.));
#7012=DIRECTION('center_axis',(0.,0.,-1.));
#7013=DIRECTION('ref_axis',(1.,0.,0.));
#7014=DIRECTION('center_axis',(0.,1.22464679914735E-16,-1.));
#7015=DIRECTION('ref_axis',(0.,1.,1.22464679914735E-16));
#7016=DIRECTION('center_axis',(0.,-1.,-1.22464679914735E-16));
#7017=DIRECTION('ref_axis',(-1.,0.,0.));
#7018=DIRECTION('center_axis',(0.,1.22464679914735E-16,-1.));
#7019=DIRECTION('ref_axis',(1.,0.,0.));
#7020=DIRECTION('',(-0.724137931034482,-0.689655172413793,-8.44583999411968E-17));
#7021=DIRECTION('center_axis',(0.,1.22464679914735E-16,-1.));
#7022=DIRECTION('ref_axis',(0.919145030018057,-0.39391929857917,-4.82412008127351E-17));
#7023=DIRECTION('',(0.,-1.,-1.22464679914735E-16));
#7024=DIRECTION('center_axis',(0.,1.22464679914735E-16,-1.));
#7025=DIRECTION('ref_axis',(0.707106781186548,0.707106781186548,8.65956056235493E-17));
#7026=DIRECTION('',(1.,2.22044604925031E-16,2.71926214689378E-32));
#7027=DIRECTION('center_axis',(0.,1.22464679914735E-16,-1.));
#7028=DIRECTION('ref_axis',(-0.393919298579166,0.919145030018059,1.12562801896381E-16));
#7029=DIRECTION('',(0.689655172413793,0.724137931034483,8.86813199382566E-17));
#7030=DIRECTION('center_axis',(0.,1.22464679914735E-16,-1.));
#7031=DIRECTION('ref_axis',(-0.928476690885259,0.371390676354104,4.54822403030224E-17));
#7032=DIRECTION('',(-2.22044604925031E-16,1.,1.22464679914735E-16));
#7033=DIRECTION('center_axis',(0.,1.22464679914735E-16,-1.));
#7034=DIRECTION('ref_axis',(-0.923879532511288,-0.382683432365088,-4.68652040532628E-17));
#7035=DIRECTION('',(-0.707106781186548,0.707106781186547,8.65956056235493E-17));
#7036=DIRECTION('center_axis',(0.,1.22464679914735E-16,-1.));
#7037=DIRECTION('ref_axis',(-0.382683432365089,-0.923879532511287,-1.1314261122877E-16));
#7038=DIRECTION('',(-1.,-2.22044604925031E-16,-2.71926214689378E-32));
#7039=DIRECTION('center_axis',(0.,-1.22464679914735E-16,1.));
#7040=DIRECTION('ref_axis',(0.363309774563981,-0.931668400079271,-1.14096472402382E-16));
#7041=DIRECTION('center_axis',(0.,1.22464679914735E-16,-1.));
#7042=DIRECTION('ref_axis',(-0.887564039861159,0.460684355220946,5.64175621038594E-17));
#7043=DIRECTION('',(-2.22044604925031E-16,1.,1.22464679914735E-16));
#7044=DIRECTION('center_axis',(0.,1.22464679914735E-16,-1.));
#7045=DIRECTION('ref_axis',(-0.923879532511288,-0.382683432365088,-4.68652040532628E-17));
#7046=DIRECTION('',(-0.707106781186547,0.707106781186548,8.65956056235494E-17));
#7047=DIRECTION('center_axis',(0.,1.22464679914735E-16,-1.));
#7048=DIRECTION('ref_axis',(-0.382683432365094,-0.923879532511285,-1.1314261122877E-16));
#7049=DIRECTION('',(-1.,0.,0.));
#7050=DIRECTION('center_axis',(0.,1.22464679914735E-16,-1.));
#7051=DIRECTION('ref_axis',(0.460684355220946,-0.887564039861159,-1.08695246045426E-16));
#7052=DIRECTION('center_axis',(0.,-1.22464679914735E-16,1.));
#7053=DIRECTION('ref_axis',(-0.931668400079272,0.363309774563981,4.44926152518725E-17));
#7054=DIRECTION('',(0.,1.,1.22464679914735E-16));
#7055=DIRECTION('center_axis',(0.,1.22464679914735E-16,-1.));
#7056=DIRECTION('ref_axis',(-0.923879532511287,-0.382683432365089,-4.68652040532629E-17));
#7057=DIRECTION('',(-0.707106781186547,0.707106781186548,8.65956056235494E-17));
#7058=DIRECTION('center_axis',(0.,1.22464679914735E-16,-1.));
#7059=DIRECTION('ref_axis',(-0.382683432365091,-0.923879532511286,-1.1314261122877E-16));
#7060=DIRECTION('',(-1.,0.,0.));
#7061=DIRECTION('center_axis',(0.,1.22464679914735E-16,-1.));
#7062=DIRECTION('ref_axis',(0.371390676354104,-0.928476690885259,-1.13705600757556E-16));
#7063=DIRECTION('center_axis',(0.,-1.22464679914735E-16,1.));
#7064=DIRECTION('ref_axis',(-2.22044604925031E-16,1.,1.22464679914735E-16));
#7065=DIRECTION('center_axis',(0.,-1.22464679914735E-16,1.));
#7066=DIRECTION('ref_axis',(1.,0.,0.));
#7067=DIRECTION('center_axis',(0.,1.22464679914735E-16,-1.));
#7068=DIRECTION('ref_axis',(-2.22044604925031E-16,1.,1.22464679914735E-16));
#7069=DIRECTION('center_axis',(0.,-1.22464679914735E-16,1.));
#7070=DIRECTION('ref_axis',(1.,0.,0.));
#7071=DIRECTION('center_axis',(0.,-1.22464679914735E-16,1.));
#7072=DIRECTION('ref_axis',(-2.22044604925031E-16,1.,1.22464679914735E-16));
#7073=DIRECTION('center_axis',(0.,1.22464679914735E-16,-1.));
#7074=DIRECTION('ref_axis',(0.,1.,1.22464679914735E-16));
#7075=DIRECTION('center_axis',(0.,1.22464679914735E-16,-1.));
#7076=DIRECTION('ref_axis',(0.,1.,1.22464679914735E-16));
#7077=DIRECTION('center_axis',(0.,0.,-1.));
#7078=DIRECTION('ref_axis',(1.,0.,0.));
#7079=DIRECTION('center_axis',(0.,-1.,-1.22464679914735E-16));
#7080=DIRECTION('ref_axis',(-1.,0.,0.));
#7081=DIRECTION('center_axis',(0.,0.,-1.));
#7082=DIRECTION('ref_axis',(1.,0.,0.));
#7083=DIRECTION('center_axis',(0.,-1.,-1.22464679914735E-16));
#7084=DIRECTION('ref_axis',(-1.,0.,0.));
#7085=DIRECTION('center_axis',(0.,-1.22464679914735E-16,1.));
#7086=DIRECTION('ref_axis',(-2.22044604925031E-16,1.,1.22464679914735E-16));
#7087=DIRECTION('',(-2.43604851491927E-16,0.707106781186547,-0.707106781186548));
#7088=DIRECTION('center_axis',(0.,1.22464679914735E-16,-1.));
#7089=DIRECTION('ref_axis',(-2.22044604925031E-16,1.,1.22464679914735E-16));
#7090=DIRECTION('center_axis',(0.,-1.22464679914735E-16,1.));
#7091=DIRECTION('ref_axis',(-2.22044604925031E-16,1.,1.22464679914735E-16));
#7092=DIRECTION('center_axis',(0.,-1.22464679914735E-16,1.));
#7093=DIRECTION('ref_axis',(-2.22044604925031E-16,1.,1.22464679914735E-16));
#7094=DIRECTION('',(0.,-1.22464679914735E-16,1.));
#7095=DIRECTION('center_axis',(0.,-1.22464679914735E-16,1.));
#7096=DIRECTION('ref_axis',(-2.22044604925031E-16,1.,1.22464679914735E-16));
#7097=DIRECTION('',(-2.43604851491927E-16,0.707106781186547,-0.707106781186548));
#7098=DIRECTION('center_axis',(0.,1.22464679914735E-16,-1.));
#7099=DIRECTION('ref_axis',(-2.22044604925031E-16,1.,1.22464679914735E-16));
#7100=DIRECTION('center_axis',(0.,-1.22464679914735E-16,1.));
#7101=DIRECTION('ref_axis',(-2.22044604925031E-16,1.,1.22464679914735E-16));
#7102=DIRECTION('center_axis',(0.,-1.22464679914735E-16,1.));
#7103=DIRECTION('ref_axis',(-2.22044604925031E-16,1.,1.22464679914735E-16));
#7104=DIRECTION('',(0.,-1.22464679914735E-16,1.));
#7105=DIRECTION('center_axis',(0.,-1.22464679914735E-16,1.));
#7106=DIRECTION('ref_axis',(1.,0.,0.));
#7107=DIRECTION('center_axis',(0.,1.22464679914735E-16,-1.));
#7108=DIRECTION('ref_axis',(1.,0.,0.));
#7109=DIRECTION('',(-0.707106781186547,-9.24446373305873E-32,0.707106781186548));
#7110=DIRECTION('center_axis',(0.,1.22464679914735E-16,-1.));
#7111=DIRECTION('ref_axis',(1.,0.,0.));
#7112=DIRECTION('center_axis',(0.,-1.22464679914735E-16,1.));
#7113=DIRECTION('ref_axis',(1.,0.,0.));
#7114=DIRECTION('',(0.,-1.22464679914735E-16,1.));
#7115=DIRECTION('center_axis',(0.,-1.22464679914735E-16,1.));
#7116=DIRECTION('ref_axis',(1.,0.,0.));
#7117=DIRECTION('center_axis',(0.,1.22464679914735E-16,-1.));
#7118=DIRECTION('ref_axis',(1.,0.,0.));
#7119=DIRECTION('',(-0.707106781186547,-9.24446373305873E-32,0.707106781186548));
#7120=DIRECTION('center_axis',(0.,1.22464679914735E-16,-1.));
#7121=DIRECTION('ref_axis',(1.,0.,0.));
#7122=DIRECTION('center_axis',(0.,-1.22464679914735E-16,1.));
#7123=DIRECTION('ref_axis',(1.,0.,0.));
#7124=DIRECTION('',(0.,-1.22464679914735E-16,1.));
#7125=DIRECTION('center_axis',(0.,1.22464679914735E-16,-1.));
#7126=DIRECTION('ref_axis',(-2.22044604925031E-16,1.,1.22464679914735E-16));
#7127=DIRECTION('',(2.43604851491927E-16,-0.707106781186547,-0.707106781186548));
#7128=DIRECTION('center_axis',(0.,1.22464679914735E-16,-1.));
#7129=DIRECTION('ref_axis',(-2.22044604925031E-16,1.,1.22464679914735E-16));
#7130=DIRECTION('center_axis',(0.,1.22464679914735E-16,-1.));
#7131=DIRECTION('ref_axis',(1.,0.,0.));
#7132=DIRECTION('',(0.724137931034482,0.689655172413793,8.44583999411968E-17));
#7133=DIRECTION('center_axis',(0.,-1.22464679914735E-16,1.));
#7134=DIRECTION('ref_axis',(0.371390676354104,-0.928476690885259,-1.13705600757556E-16));
#7135=DIRECTION('',(1.,0.,0.));
#7136=DIRECTION('center_axis',(0.,-1.22464679914735E-16,1.));
#7137=DIRECTION('ref_axis',(-0.382683432365091,-0.923879532511286,-1.1314261122877E-16));
#7138=DIRECTION('',(0.707106781186547,-0.707106781186548,-8.65956056235494E-17));
#7139=DIRECTION('center_axis',(0.,-1.22464679914735E-16,1.));
#7140=DIRECTION('ref_axis',(-0.923879532511287,-0.382683432365089,-4.68652040532629E-17));
#7141=DIRECTION('',(0.,-1.,-1.22464679914735E-16));
#7142=DIRECTION('center_axis',(0.,1.22464679914735E-16,-1.));
#7143=DIRECTION('ref_axis',(-0.931668400079272,0.363309774563981,4.44926152518725E-17));
#7144=DIRECTION('center_axis',(0.,-1.22464679914735E-16,1.));
#7145=DIRECTION('ref_axis',(0.460684355220946,-0.887564039861159,-1.08695246045426E-16));
#7146=DIRECTION('',(1.,0.,0.));
#7147=DIRECTION('center_axis',(0.,-1.22464679914735E-16,1.));
#7148=DIRECTION('ref_axis',(-0.382683432365094,-0.923879532511285,-1.1314261122877E-16));
#7149=DIRECTION('',(0.707106781186547,-0.707106781186548,-8.65956056235494E-17));
#7150=DIRECTION('center_axis',(0.,-1.22464679914735E-16,1.));
#7151=DIRECTION('ref_axis',(-0.923879532511288,-0.382683432365088,-4.68652040532628E-17));
#7152=DIRECTION('',(2.22044604925031E-16,-1.,-1.22464679914735E-16));
#7153=DIRECTION('center_axis',(0.,-1.22464679914735E-16,1.));
#7154=DIRECTION('ref_axis',(-0.887564039861159,0.460684355220946,5.64175621038594E-17));
#7155=DIRECTION('center_axis',(0.,1.22464679914735E-16,-1.));
#7156=DIRECTION('ref_axis',(0.363309774563981,-0.931668400079271,-1.14096472402382E-16));
#7157=DIRECTION('',(1.,2.22044604925031E-16,2.71926214689378E-32));
#7158=DIRECTION('center_axis',(0.,-1.22464679914735E-16,1.));
#7159=DIRECTION('ref_axis',(-0.382683432365089,-0.923879532511287,-1.1314261122877E-16));
#7160=DIRECTION('',(0.707106781186548,-0.707106781186547,-8.65956056235493E-17));
#7161=DIRECTION('center_axis',(0.,-1.22464679914735E-16,1.));
#7162=DIRECTION('ref_axis',(-0.923879532511287,-0.382683432365088,-4.68652040532628E-17));
#7163=DIRECTION('',(2.22044604925031E-16,-1.,-1.22464679914735E-16));
#7164=DIRECTION('center_axis',(0.,-1.22464679914735E-16,1.));
#7165=DIRECTION('ref_axis',(-0.928476690885259,0.371390676354104,4.54822403030224E-17));
#7166=DIRECTION('',(-0.689655172413793,-0.724137931034483,-8.86813199382566E-17));
#7167=DIRECTION('center_axis',(0.,-1.22464679914735E-16,1.));
#7168=DIRECTION('ref_axis',(-0.393919298579166,0.919145030018059,1.12562801896381E-16));
#7169=DIRECTION('',(-1.,-2.22044604925031E-16,-2.71926214689378E-32));
#7170=DIRECTION('center_axis',(0.,-1.22464679914735E-16,1.));
#7171=DIRECTION('ref_axis',(0.707106781186548,0.707106781186548,8.65956056235493E-17));
#7172=DIRECTION('',(0.,1.,1.22464679914735E-16));
#7173=DIRECTION('center_axis',(0.,-1.22464679914735E-16,1.));
#7174=DIRECTION('ref_axis',(0.919145030018057,-0.39391929857917,-4.82412008127351E-17));
#7175=DIRECTION('center_axis',(0.,1.22464679914735E-16,-1.));
#7176=DIRECTION('ref_axis',(-2.22044604925031E-16,1.,1.22464679914735E-16));
#7177=DIRECTION('center_axis',(0.,1.22464679914735E-16,-1.));
#7178=DIRECTION('ref_axis',(1.,0.,0.));
#7179=DIRECTION('center_axis',(0.,-1.22464679914735E-16,1.));
#7180=DIRECTION('ref_axis',(1.,0.,0.));
#7181=DIRECTION('center_axis',(0.,1.22464679914735E-16,-1.));
#7182=DIRECTION('ref_axis',(1.,0.,0.));
#7183=DIRECTION('center_axis',(0.,1.22464679914735E-16,-1.));
#7184=DIRECTION('ref_axis',(-2.22044604925031E-16,1.,1.22464679914735E-16));
#7185=DIRECTION('',(2.43604851491927E-16,-0.707106781186547,-0.707106781186548));
#7186=DIRECTION('center_axis',(0.,1.22464679914735E-16,-1.));
#7187=DIRECTION('ref_axis',(1.,0.,0.));
#7188=DIRECTION('',(0.707106781186547,-1.73191211247099E-16,0.707106781186548));
#7189=DIRECTION('center_axis',(0.,1.22464679914735E-16,-1.));
#7190=DIRECTION('ref_axis',(1.,0.,0.));
#7191=DIRECTION('',(0.707106781186547,-1.73191211247099E-16,0.707106781186548));
#7192=DIRECTION('center_axis',(0.487659849094173,-0.512042841548881,-0.707106781186545));
#7193=DIRECTION('ref_axis',(0.823212785915304,-6.95272347095421E-17,0.567732955803662));
#7194=DIRECTION('',(-0.48765984909417,0.512042841548878,-0.70710678118655));
#7195=DIRECTION('',(0.48765984909417,-0.512042841548877,0.707106781186549));
#7196=DIRECTION('',(-0.724137931034482,-0.689655172413793,-8.44583999411968E-17));
#7197=DIRECTION('center_axis',(0.,-1.22464679914735E-16,1.));
#7198=DIRECTION('ref_axis',(0.371390676354104,-0.928476690885259,-1.13705600757556E-16));
#7199=DIRECTION('center_axis',(0.,1.22464679914735E-16,-1.));
#7200=DIRECTION('ref_axis',(0.371390676354104,-0.928476690885259,-1.13705600757556E-16));
#7201=DIRECTION('',(0.,0.707106781186549,-0.707106781186546));
#7202=DIRECTION('center_axis',(0.,-0.707106781186549,-0.707106781186546));
#7203=DIRECTION('ref_axis',(1.,0.,0.));
#7204=DIRECTION('',(0.,0.707106781186546,-0.707106781186549));
#7205=DIRECTION('',(-1.,0.,0.));
#7206=DIRECTION('center_axis',(0.,-1.22464679914735E-16,1.));
#7207=DIRECTION('ref_axis',(-0.382683432365091,-0.923879532511286,-1.1314261122877E-16));
#7208=DIRECTION('center_axis',(0.,1.22464679914735E-16,-1.));
#7209=DIRECTION('ref_axis',(-0.382683432365091,-0.923879532511286,-1.1314261122877E-16));
#7210=DIRECTION('',(0.499999999999999,0.499999999999995,-0.707106781186552));
#7211=DIRECTION('center_axis',(-0.500000000000001,-0.5,-0.707106781186547));
#7212=DIRECTION('ref_axis',(0.816496580927725,7.0705015914994E-17,-0.577350269189627));
#7213=DIRECTION('',(0.499999999999998,0.5,-0.707106781186549));
#7214=DIRECTION('',(-0.707106781186547,0.707106781186548,8.65956056235494E-17));
#7215=DIRECTION('center_axis',(0.,-1.22464679914735E-16,1.));
#7216=DIRECTION('ref_axis',(-0.923879532511287,-0.382683432365089,-4.68652040532629E-17));
#7217=DIRECTION('center_axis',(0.,1.22464679914735E-16,-1.));
#7218=DIRECTION('ref_axis',(-0.923879532511287,-0.382683432365089,-4.68652040532629E-17));
#7219=DIRECTION('',(0.707106781186547,8.65956056235493E-17,-0.707106781186547));
#7220=DIRECTION('center_axis',(-0.707106781186548,8.65956056235493E-17,
-0.707106781186548));
#7221=DIRECTION('ref_axis',(0.707106781186548,8.65956056235493E-17,-0.707106781186548));
#7222=DIRECTION('',(0.707106781186547,8.65956056235494E-17,-0.707106781186548));
#7223=DIRECTION('',(0.,1.,1.22464679914735E-16));
#7224=DIRECTION('center_axis',(0.,1.22464679914735E-16,-1.));
#7225=DIRECTION('ref_axis',(-0.931668400079272,0.363309774563981,4.44926152518725E-17));
#7226=DIRECTION('',(-0.578253353382651,0.406968130572547,-0.707106781186551));
#7227=DIRECTION('center_axis',(0.,-1.22464679914735E-16,1.));
#7228=DIRECTION('ref_axis',(-0.931668400079272,0.363309774563981,4.44926152518725E-17));
#7229=DIRECTION('center_axis',(0.,-1.22464679914735E-16,1.));
#7230=DIRECTION('ref_axis',(0.460684355220946,-0.887564039861159,-1.08695246045426E-16));
#7231=DIRECTION('center_axis',(0.,1.22464679914735E-16,-1.));
#7232=DIRECTION('ref_axis',(0.460684355220946,-0.887564039861159,-1.08695246045426E-16));
#7233=DIRECTION('',(0.,0.707106781186549,-0.707106781186546));
#7234=DIRECTION('center_axis',(0.,-0.707106781186549,-0.707106781186546));
#7235=DIRECTION('ref_axis',(1.,0.,0.));
#7236=DIRECTION('',(0.,0.707106781186546,-0.707106781186549));
#7237=DIRECTION('',(-1.,0.,0.));
#7238=DIRECTION('center_axis',(0.,-1.22464679914735E-16,1.));
#7239=DIRECTION('ref_axis',(-0.382683432365094,-0.923879532511285,-1.1314261122877E-16));
#7240=DIRECTION('center_axis',(0.,1.22464679914735E-16,-1.));
#7241=DIRECTION('ref_axis',(-0.382683432365094,-0.923879532511285,-1.1314261122877E-16));
#7242=DIRECTION('',(0.500000000000001,0.499999999999995,-0.707106781186551));
#7243=DIRECTION('center_axis',(-0.500000000000001,-0.5,-0.707106781186547));
#7244=DIRECTION('ref_axis',(0.816496580927725,7.0705015914994E-17,-0.577350269189627));
#7245=DIRECTION('',(0.499999999999999,0.499999999999999,-0.707106781186548));
#7246=DIRECTION('',(-0.707106781186547,0.707106781186548,8.65956056235494E-17));
#7247=DIRECTION('center_axis',(0.,-1.22464679914735E-16,1.));
#7248=DIRECTION('ref_axis',(-0.923879532511287,-0.382683432365088,-4.68652040532628E-17));
#7249=DIRECTION('center_axis',(0.,1.22464679914735E-16,-1.));
#7250=DIRECTION('ref_axis',(-0.923879532511288,-0.382683432365088,-4.68652040532628E-17));
#7251=DIRECTION('',(0.707106781186549,3.22678052299109E-15,-0.707106781186546));
#7252=DIRECTION('center_axis',(-0.707106781186549,-7.04136402448287E-17,
-0.707106781186546));
#7253=DIRECTION('ref_axis',(0.707106781186546,8.65956056235495E-17,-0.707106781186549));
#7254=DIRECTION('',(-2.22044604925031E-16,1.,1.22464679914735E-16));
#7255=DIRECTION('',(0.707106781186546,8.65956056235495E-17,-0.707106781186549));
#7256=DIRECTION('center_axis',(0.,-1.22464679914735E-16,1.));
#7257=DIRECTION('ref_axis',(-0.887564039861159,0.460684355220946,5.64175621038594E-17));
#7258=DIRECTION('center_axis',(0.,1.22464679914735E-16,-1.));
#7259=DIRECTION('ref_axis',(-0.887564039861159,0.460684355220946,5.64175621038594E-17));
#7260=DIRECTION('',(0.406968130572545,-0.578253353382658,-0.707106781186547));
#7261=DIRECTION('center_axis',(0.,1.22464679914735E-16,-1.));
#7262=DIRECTION('ref_axis',(0.363309774563981,-0.931668400079272,-1.14096472402382E-16));
#7263=DIRECTION('center_axis',(0.,-1.22464679914735E-16,1.));
#7264=DIRECTION('ref_axis',(0.363309774563981,-0.931668400079271,-1.14096472402382E-16));
#7265=DIRECTION('',(0.,0.707106781186546,-0.707106781186549));
#7266=DIRECTION('center_axis',(1.57009245868378E-16,-0.707106781186547,
-0.707106781186548));
#7267=DIRECTION('ref_axis',(1.,-2.71926214689378E-32,2.22044604925031E-16));
#7268=DIRECTION('',(-1.,-2.22044604925031E-16,-2.71926214689378E-32));
#7269=DIRECTION('',(0.,0.707106781186548,-0.707106781186547));
#7270=DIRECTION('center_axis',(0.,-1.22464679914735E-16,1.));
#7271=DIRECTION('ref_axis',(-0.382683432365089,-0.923879532511287,-1.1314261122877E-16));
#7272=DIRECTION('center_axis',(0.,1.22464679914735E-16,-1.));
#7273=DIRECTION('ref_axis',(-0.382683432365089,-0.923879532511287,-1.1314261122877E-16));
#7274=DIRECTION('',(0.499999999999999,0.500000000000001,-0.707106781186548));
#7275=DIRECTION('center_axis',(-0.500000000000001,-0.500000000000002,-0.707106781186545));
#7276=DIRECTION('ref_axis',(0.816496580927724,7.07050159149941E-17,-0.577350269189628));
#7277=DIRECTION('',(-0.707106781186548,0.707106781186547,8.65956056235493E-17));
#7278=DIRECTION('',(0.499999999999997,0.500000000000001,-0.707106781186549));
#7279=DIRECTION('center_axis',(0.,-1.22464679914735E-16,1.));
#7280=DIRECTION('ref_axis',(-0.923879532511287,-0.382683432365088,-4.68652040532628E-17));
#7281=DIRECTION('center_axis',(0.,1.22464679914735E-16,-1.));
#7282=DIRECTION('ref_axis',(-0.923879532511287,-0.382683432365088,-4.68652040532628E-17));
#7283=DIRECTION('',(0.707106781186546,8.65956056235495E-17,-0.707106781186549));
#7284=DIRECTION('center_axis',(-0.707106781186549,-7.04136402448287E-17,
-0.707106781186546));
#7285=DIRECTION('ref_axis',(0.707106781186546,8.65956056235495E-17,-0.707106781186549));
#7286=DIRECTION('',(-2.22044604925031E-16,1.,1.22464679914735E-16));
#7287=DIRECTION('',(0.707106781186546,8.65956056235495E-17,-0.707106781186549));
#7288=DIRECTION('center_axis',(0.,-1.22464679914735E-16,1.));
#7289=DIRECTION('ref_axis',(-0.928476690885259,0.371390676354104,4.54822403030224E-17));
#7290=DIRECTION('center_axis',(0.,1.22464679914735E-16,-1.));
#7291=DIRECTION('ref_axis',(-0.928476690885259,0.371390676354104,4.54822403030224E-17));
#7292=DIRECTION('',(0.512042841548877,-0.487659849094171,-0.707106781186549));
#7293=DIRECTION('center_axis',(-0.512042841548879,0.487659849094171,-0.707106781186547));
#7294=DIRECTION('ref_axis',(0.809942121543021,7.1826736412027E-17,-0.586509812151843));
#7295=DIRECTION('',(0.689655172413793,0.724137931034483,8.86813199382566E-17));
#7296=DIRECTION('',(0.512042841548878,-0.487659849094171,-0.707106781186548));
#7297=DIRECTION('center_axis',(0.,-1.22464679914735E-16,1.));
#7298=DIRECTION('ref_axis',(-0.393919298579166,0.919145030018059,1.12562801896381E-16));
#7299=DIRECTION('center_axis',(0.,1.22464679914735E-16,-1.));
#7300=DIRECTION('ref_axis',(-0.393919298579166,0.919145030018059,1.12562801896381E-16));
#7301=DIRECTION('',(0.,-0.707106781186547,-0.707106781186548));
#7302=DIRECTION('center_axis',(-1.57009245868377E-16,0.707106781186547,
-0.707106781186548));
#7303=DIRECTION('ref_axis',(1.,2.71926214689378E-32,-2.22044604925031E-16));
#7304=DIRECTION('',(1.,2.22044604925031E-16,2.71926214689378E-32));
#7305=DIRECTION('',(0.,-0.707106781186549,-0.707106781186546));
#7306=DIRECTION('center_axis',(0.,-1.22464679914735E-16,1.));
#7307=DIRECTION('ref_axis',(0.707106781186547,0.707106781186547,8.65956056235493E-17));
#7308=DIRECTION('center_axis',(0.,1.22464679914735E-16,-1.));
#7309=DIRECTION('ref_axis',(0.707106781186548,0.707106781186547,8.65956056235493E-17));
#7310=DIRECTION('',(-0.707106781186547,-6.98450623718338E-16,-0.707106781186548));
#7311=DIRECTION('center_axis',(0.707106781186548,8.65956056235493E-17,-0.707106781186547));
#7312=DIRECTION('ref_axis',(0.707106781186547,-8.65956056235494E-17,0.707106781186548));
#7313=DIRECTION('',(-0.707106781186547,8.65956056235494E-17,-0.707106781186548));
#7314=DIRECTION('',(0.,-1.,-1.22464679914735E-16));
#7315=DIRECTION('center_axis',(0.,-1.22464679914735E-16,1.));
#7316=DIRECTION('ref_axis',(0.919145030018057,-0.39391929857917,-4.82412008127351E-17));
#7317=DIRECTION('center_axis',(0.,1.22464679914735E-16,-1.));
#7318=DIRECTION('ref_axis',(0.919145030018057,-0.39391929857917,-4.82412008127351E-17));
#7319=DIRECTION('center_axis',(1.,2.22044604925031E-16,2.71926214689378E-32));
#7320=DIRECTION('ref_axis',(2.22044604925031E-16,-1.,-1.22464679914735E-16));
#7321=DIRECTION('',(0.,1.22464679914735E-16,-1.));
#7322=DIRECTION('',(2.22044604925031E-16,-1.,-1.22464679914735E-16));
#7323=DIRECTION('',(0.,-1.22464679914735E-16,1.));
#7324=DIRECTION('center_axis',(0.,1.22464679914735E-16,-1.));
#7325=DIRECTION('ref_axis',(-0.923879532511288,-0.382683432365088,-4.68652040532628E-17));
#7326=DIRECTION('',(0.,-1.22464679914735E-16,1.));
#7327=DIRECTION('center_axis',(0.,-1.22464679914735E-16,1.));
#7328=DIRECTION('ref_axis',(-0.923879532511288,-0.382683432365088,-4.68652040532628E-17));
#7329=DIRECTION('center_axis',(-0.707106781186548,-0.707106781186547,-8.65956056235492E-17));
#7330=DIRECTION('ref_axis',(-0.707106781186547,0.707106781186548,8.65956056235494E-17));
#7331=DIRECTION('',(0.,1.22464679914735E-16,-1.));
#7332=DIRECTION('',(0.707106781186547,-0.707106781186548,-8.65956056235494E-17));
#7333=DIRECTION('center_axis',(0.,1.22464679914735E-16,-1.));
#7334=DIRECTION('ref_axis',(-0.382683432365094,-0.923879532511285,-1.1314261122877E-16));
#7335=DIRECTION('',(0.,-1.22464679914735E-16,1.));
#7336=DIRECTION('center_axis',(0.,-1.22464679914735E-16,1.));
#7337=DIRECTION('ref_axis',(-0.382683432365094,-0.923879532511285,-1.1314261122877E-16));
#7338=DIRECTION('center_axis',(0.,-1.,-1.22464679914735E-16));
#7339=DIRECTION('ref_axis',(-1.,0.,0.));
#7340=DIRECTION('',(0.,1.22464679914735E-16,-1.));
#7341=DIRECTION('',(1.,0.,0.));
#7342=DIRECTION('center_axis',(0.,1.22464679914735E-16,-1.));
#7343=DIRECTION('ref_axis',(0.460684355220946,-0.887564039861159,-1.08695246045426E-16));
#7344=DIRECTION('',(0.,-1.22464679914735E-16,1.));
#7345=DIRECTION('center_axis',(0.,-1.22464679914735E-16,1.));
#7346=DIRECTION('ref_axis',(0.460684355220946,-0.887564039861159,-1.08695246045426E-16));
#7347=DIRECTION('center_axis',(0.,1.22464679914735E-16,-1.));
#7348=DIRECTION('ref_axis',(-0.931668400079272,0.363309774563981,4.44926152518725E-17));
#7349=DIRECTION('',(0.,1.22464679914735E-16,-1.));
#7350=DIRECTION('center_axis',(0.,1.22464679914735E-16,-1.));
#7351=DIRECTION('ref_axis',(-0.931668400079272,0.363309774563981,4.44926152518725E-17));
#7352=DIRECTION('center_axis',(-1.,0.,0.));
#7353=DIRECTION('ref_axis',(0.,1.,1.22464679914735E-16));
#7354=DIRECTION('',(0.,1.22464679914735E-16,-1.));
#7355=DIRECTION('',(0.,-1.,-1.22464679914735E-16));
#7356=DIRECTION('center_axis',(0.,1.22464679914735E-16,-1.));
#7357=DIRECTION('ref_axis',(-0.923879532511287,-0.382683432365089,-4.68652040532629E-17));
#7358=DIRECTION('',(0.,-1.22464679914735E-16,1.));
#7359=DIRECTION('center_axis',(0.,-1.22464679914735E-16,1.));
#7360=DIRECTION('ref_axis',(-0.923879532511287,-0.382683432365089,-4.68652040532629E-17));
#7361=DIRECTION('center_axis',(-0.707106781186548,-0.707106781186547,-8.65956056235493E-17));
#7362=DIRECTION('ref_axis',(-0.707106781186547,0.707106781186548,8.65956056235494E-17));
#7363=DIRECTION('',(0.,1.22464679914735E-16,-1.));
#7364=DIRECTION('',(0.707106781186547,-0.707106781186548,-8.65956056235494E-17));
#7365=DIRECTION('center_axis',(0.,1.22464679914735E-16,-1.));
#7366=DIRECTION('ref_axis',(-0.382683432365091,-0.923879532511286,-1.1314261122877E-16));
#7367=DIRECTION('',(0.,-1.22464679914735E-16,1.));
#7368=DIRECTION('center_axis',(0.,-1.22464679914735E-16,1.));
#7369=DIRECTION('ref_axis',(-0.382683432365091,-0.923879532511286,-1.1314261122877E-16));
#7370=DIRECTION('center_axis',(0.,-1.,-1.22464679914735E-16));
#7371=DIRECTION('ref_axis',(-1.,0.,0.));
#7372=DIRECTION('',(0.,1.22464679914735E-16,-1.));
#7373=DIRECTION('',(1.,0.,0.));
#7374=DIRECTION('center_axis',(0.,1.22464679914735E-16,-1.));
#7375=DIRECTION('ref_axis',(0.371390676354104,-0.928476690885259,-1.13705600757556E-16));
#7376=DIRECTION('',(0.,-1.22464679914735E-16,1.));
#7377=DIRECTION('center_axis',(0.,-1.22464679914735E-16,1.));
#7378=DIRECTION('ref_axis',(0.371390676354104,-0.928476690885259,-1.13705600757556E-16));
#7379=DIRECTION('center_axis',(0.689655172413793,-0.724137931034482,-8.86813199382566E-17));
#7380=DIRECTION('ref_axis',(-0.724137931034482,-0.689655172413793,-8.44583999411968E-17));
#7381=DIRECTION('',(0.,1.22464679914735E-16,-1.));
#7382=DIRECTION('',(0.724137931034482,0.689655172413793,8.44583999411968E-17));
#7383=DIRECTION('center_axis',(0.487659849094172,-0.512042841548881,0.707106781186545));
#7384=DIRECTION('ref_axis',(-0.823212785915305,-6.9527234709542E-17,0.567732955803662));
#7385=DIRECTION('',(0.487659849094171,-0.512042841548877,-0.707106781186549));
#7386=DIRECTION('',(-0.487659849094171,0.512042841548877,0.707106781186549));
#7387=DIRECTION('center_axis',(0.,1.22464679914735E-16,-1.));
#7388=DIRECTION('ref_axis',(0.371390676354104,-0.928476690885259,-1.13705600757556E-16));
#7389=DIRECTION('',(0.,-0.707106781186549,-0.707106781186546));
#7390=DIRECTION('center_axis',(0.,-0.707106781186549,0.707106781186546));
#7391=DIRECTION('ref_axis',(-1.,0.,0.));
#7392=DIRECTION('',(0.,-0.707106781186546,-0.707106781186549));
#7393=DIRECTION('center_axis',(0.,1.22464679914735E-16,-1.));
#7394=DIRECTION('ref_axis',(-0.382683432365091,-0.923879532511286,-1.1314261122877E-16));
#7395=DIRECTION('',(-0.499999999999999,-0.499999999999995,-0.707106781186552));
#7396=DIRECTION('center_axis',(-0.5,-0.5,0.707106781186548));
#7397=DIRECTION('ref_axis',(-0.816496580927726,7.07050159149938E-17,-0.577350269189626));
#7398=DIRECTION('',(-0.5,-0.499999999999999,-0.707106781186548));
#7399=DIRECTION('center_axis',(0.,1.22464679914735E-16,-1.));
#7400=DIRECTION('ref_axis',(-0.923879532511287,-0.382683432365089,-4.68652040532629E-17));
#7401=DIRECTION('',(-0.707106781186547,8.65956056235493E-17,-0.707106781186547));
#7402=DIRECTION('center_axis',(-0.707106781186548,-8.65956056235493E-17,
0.707106781186548));
#7403=DIRECTION('ref_axis',(-0.707106781186548,8.65956056235493E-17,-0.707106781186548));
#7404=DIRECTION('',(-0.707106781186547,8.65956056235494E-17,-0.707106781186548));
#7405=DIRECTION('center_axis',(0.,-1.22464679914735E-16,1.));
#7406=DIRECTION('ref_axis',(-0.931668400079272,0.363309774563981,4.44926152518725E-17));
#7407=DIRECTION('',(0.578253353382651,-0.406968130572547,-0.707106781186551));
#7408=DIRECTION('center_axis',(0.,1.22464679914735E-16,-1.));
#7409=DIRECTION('ref_axis',(0.460684355220946,-0.887564039861159,-1.08695246045426E-16));
#7410=DIRECTION('',(0.,-0.707106781186549,-0.707106781186546));
#7411=DIRECTION('center_axis',(0.,-0.707106781186549,0.707106781186546));
#7412=DIRECTION('ref_axis',(-1.,0.,0.));
#7413=DIRECTION('',(0.,-0.707106781186546,-0.707106781186549));
#7414=DIRECTION('center_axis',(0.,1.22464679914735E-16,-1.));
#7415=DIRECTION('ref_axis',(-0.382683432365094,-0.923879532511285,-1.1314261122877E-16));
#7416=DIRECTION('',(-0.500000000000001,-0.499999999999994,-0.707106781186551));
#7417=DIRECTION('center_axis',(-0.500000000000001,-0.5,0.707106781186546));
#7418=DIRECTION('ref_axis',(-0.816496580927725,7.0705015914994E-17,-0.577350269189627));
#7419=DIRECTION('',(-0.499999999999999,-0.499999999999999,-0.707106781186549));
#7420=DIRECTION('center_axis',(0.,1.22464679914735E-16,-1.));
#7421=DIRECTION('ref_axis',(-0.923879532511287,-0.382683432365088,-4.68652040532628E-17));
#7422=DIRECTION('',(-0.707106781186549,-3.05358931174399E-15,-0.707106781186546));
#7423=DIRECTION('center_axis',(-0.707106781186549,-2.43604851491927E-16,
0.707106781186546));
#7424=DIRECTION('ref_axis',(-0.707106781186546,8.65956056235495E-17,-0.707106781186549));
#7425=DIRECTION('',(-0.707106781186546,8.65956056235495E-17,-0.707106781186549));
#7426=DIRECTION('center_axis',(0.,1.22464679914735E-16,-1.));
#7427=DIRECTION('ref_axis',(-0.887564039861159,0.460684355220946,5.64175621038594E-17));
#7428=DIRECTION('',(-0.406968130572545,0.578253353382658,-0.707106781186547));
#7429=DIRECTION('center_axis',(0.,-1.22464679914735E-16,1.));
#7430=DIRECTION('ref_axis',(-0.887564039861159,0.460684355220946,5.64175621038594E-17));
#7431=DIRECTION('center_axis',(0.,-1.22464679914735E-16,1.));
#7432=DIRECTION('ref_axis',(0.363309774563981,-0.931668400079272,-1.14096472402382E-16));
#7433=DIRECTION('',(0.,-0.707106781186546,-0.707106781186549));
#7434=DIRECTION('center_axis',(0.,1.22464679914735E-16,-1.));
#7435=DIRECTION('ref_axis',(0.363309774563981,-0.931668400079271,-1.14096472402382E-16));
#7436=DIRECTION('center_axis',(1.57009245868378E-16,-0.707106781186548,
0.707106781186547));
#7437=DIRECTION('ref_axis',(-1.,-2.71926214689378E-32,2.22044604925031E-16));
#7438=DIRECTION('',(0.,-0.707106781186547,-0.707106781186548));
#7439=DIRECTION('',(1.,2.22044604925031E-16,2.71926214689378E-32));
#7440=DIRECTION('center_axis',(0.,1.22464679914735E-16,-1.));
#7441=DIRECTION('ref_axis',(-0.382683432365089,-0.923879532511287,-1.1314261122877E-16));
#7442=DIRECTION('',(-0.499999999999999,-0.499999999999999,-0.707106781186549));
#7443=DIRECTION('center_axis',(0.,-1.22464679914735E-16,1.));
#7444=DIRECTION('ref_axis',(-0.382683432365089,-0.923879532511287,-1.1314261122877E-16));
#7445=DIRECTION('center_axis',(-0.499999999999997,-0.499999999999998,0.707106781186551));
#7446=DIRECTION('ref_axis',(-0.816496580927729,7.07050159149933E-17,-0.577350269189622));
#7447=DIRECTION('',(-0.500000000000002,-0.500000000000005,-0.707106781186543));
#7448=DIRECTION('',(0.707106781186548,-0.707106781186547,-8.65956056235493E-17));
#7449=DIRECTION('center_axis',(0.,1.22464679914735E-16,-1.));
#7450=DIRECTION('ref_axis',(-0.923879532511287,-0.382683432365088,-4.68652040532628E-17));
#7451=DIRECTION('',(-0.707106781186546,8.65956056235495E-17,-0.707106781186549));
#7452=DIRECTION('center_axis',(0.,-1.22464679914735E-16,1.));
#7453=DIRECTION('ref_axis',(-0.923879532511287,-0.382683432365088,-4.68652040532628E-17));
#7454=DIRECTION('center_axis',(-0.707106781186549,-2.43604851491927E-16,
0.707106781186546));
#7455=DIRECTION('ref_axis',(-0.707106781186546,8.65956056235495E-17,-0.707106781186549));
#7456=DIRECTION('',(-0.707106781186546,8.65956056235495E-17,-0.707106781186549));
#7457=DIRECTION('',(2.22044604925031E-16,-1.,-1.22464679914735E-16));
#7458=DIRECTION('center_axis',(0.,1.22464679914735E-16,-1.));
#7459=DIRECTION('ref_axis',(-0.928476690885259,0.371390676354104,4.54822403030224E-17));
#7460=DIRECTION('',(-0.512042841548877,0.487659849094171,-0.707106781186549));
#7461=DIRECTION('center_axis',(0.,-1.22464679914735E-16,1.));
#7462=DIRECTION('ref_axis',(-0.928476690885259,0.371390676354104,4.54822403030224E-17));
#7463=DIRECTION('center_axis',(-0.51204284154888,0.487659849094172,0.707106781186546));
#7464=DIRECTION('ref_axis',(-0.80994212154302,7.18267364120272E-17,-0.586509812151845));
#7465=DIRECTION('',(-0.512042841548877,0.48765984909417,-0.707106781186549));
#7466=DIRECTION('',(-0.689655172413793,-0.724137931034483,-8.86813199382566E-17));
#7467=DIRECTION('center_axis',(0.,1.22464679914735E-16,-1.));
#7468=DIRECTION('ref_axis',(-0.393919298579166,0.919145030018059,1.12562801896381E-16));
#7469=DIRECTION('',(0.,0.707106781186548,-0.707106781186547));
#7470=DIRECTION('center_axis',(0.,-1.22464679914735E-16,1.));
#7471=DIRECTION('ref_axis',(-0.393919298579166,0.919145030018059,1.12562801896381E-16));
#7472=DIRECTION('center_axis',(-1.57009245868377E-16,0.707106781186547,
0.707106781186548));
#7473=DIRECTION('ref_axis',(-1.,2.71926214689378E-32,-2.22044604925031E-16));
#7474=DIRECTION('',(0.,0.707106781186549,-0.707106781186546));
#7475=DIRECTION('',(-1.,-2.22044604925031E-16,-2.71926214689378E-32));
#7476=DIRECTION('center_axis',(0.,1.22464679914735E-16,-1.));
#7477=DIRECTION('ref_axis',(0.707106781186547,0.707106781186547,8.65956056235493E-17));
#7478=DIRECTION('',(0.707106781186547,8.71641834965437E-16,-0.707106781186548));
#7479=DIRECTION('center_axis',(0.,-1.22464679914735E-16,1.));
#7480=DIRECTION('ref_axis',(0.707106781186548,0.707106781186547,8.65956056235493E-17));
#7481=DIRECTION('center_axis',(0.707106781186548,-8.65956056235493E-17,
0.707106781186547));
#7482=DIRECTION('ref_axis',(-0.707106781186547,-8.65956056235494E-17,0.707106781186548));
#7483=DIRECTION('',(0.707106781186547,8.65956056235494E-17,-0.707106781186548));
#7484=DIRECTION('',(0.,1.,1.22464679914735E-16));
#7485=DIRECTION('center_axis',(0.,1.22464679914735E-16,-1.));
#7486=DIRECTION('ref_axis',(0.919145030018057,-0.39391929857917,-4.82412008127351E-17));
#7487=DIRECTION('center_axis',(0.,-1.22464679914735E-16,1.));
#7488=DIRECTION('ref_axis',(0.919145030018057,-0.39391929857917,-4.82412008127351E-17));
#7489=DIRECTION('center_axis',(0.,-1.22464679914735E-16,1.));
#7490=DIRECTION('ref_axis',(0.363309774563981,-0.931668400079271,-1.14096472402382E-16));
#7491=DIRECTION('',(0.,1.22464679914735E-16,-1.));
#7492=DIRECTION('',(0.,1.22464679914735E-16,-1.));
#7493=DIRECTION('center_axis',(-2.22044604925031E-16,1.,1.22464679914735E-16));
#7494=DIRECTION('ref_axis',(1.,2.22044604925031E-16,2.71926214689378E-32));
#7495=DIRECTION('',(0.,-1.22464679914735E-16,1.));
#7496=DIRECTION('center_axis',(0.,1.22464679914735E-16,-1.));
#7497=DIRECTION('ref_axis',(-0.382683432365089,-0.923879532511287,-1.1314261122877E-16));
#7498=DIRECTION('',(0.,1.22464679914735E-16,-1.));
#7499=DIRECTION('center_axis',(0.707106781186547,0.707106781186548,8.65956056235494E-17));
#7500=DIRECTION('ref_axis',(0.707106781186548,-0.707106781186547,-8.65956056235493E-17));
#7501=DIRECTION('',(0.,-1.22464679914735E-16,1.));
#7502=DIRECTION('center_axis',(0.,1.22464679914735E-16,-1.));
#7503=DIRECTION('ref_axis',(-0.923879532511287,-0.382683432365088,-4.68652040532628E-17));
#7504=DIRECTION('',(0.,1.22464679914735E-16,-1.));
#7505=DIRECTION('center_axis',(1.,2.22044604925031E-16,2.71926214689378E-32));
#7506=DIRECTION('ref_axis',(2.22044604925031E-16,-1.,-1.22464679914735E-16));
#7507=DIRECTION('',(0.,-1.22464679914735E-16,1.));
#7508=DIRECTION('center_axis',(0.,1.22464679914735E-16,-1.));
#7509=DIRECTION('ref_axis',(-0.928476690885259,0.371390676354104,4.54822403030224E-17));
#7510=DIRECTION('',(0.,1.22464679914735E-16,-1.));
#7511=DIRECTION('center_axis',(0.724137931034483,-0.689655172413793,-8.44583999411968E-17));
#7512=DIRECTION('ref_axis',(-0.689655172413793,-0.724137931034483,-8.86813199382566E-17));
#7513=DIRECTION('',(0.,-1.22464679914735E-16,1.));
#7514=DIRECTION('center_axis',(0.,1.22464679914735E-16,-1.));
#7515=DIRECTION('ref_axis',(-0.393919298579166,0.919145030018059,1.12562801896381E-16));
#7516=DIRECTION('',(0.,1.22464679914735E-16,-1.));
#7517=DIRECTION('center_axis',(2.22044604925031E-16,-1.,-1.22464679914735E-16));
#7518=DIRECTION('ref_axis',(-1.,-2.22044604925031E-16,-2.71926214689378E-32));
#7519=DIRECTION('',(0.,1.22464679914735E-16,-1.));
#7520=DIRECTION('center_axis',(0.,1.22464679914735E-16,-1.));
#7521=DIRECTION('ref_axis',(0.707106781186547,0.707106781186548,8.65956056235493E-17));
#7522=DIRECTION('',(0.,1.22464679914735E-16,-1.));
#7523=DIRECTION('center_axis',(1.,0.,0.));
#7524=DIRECTION('ref_axis',(0.,-1.,-1.22464679914735E-16));
#7525=DIRECTION('',(0.,-1.22464679914735E-16,1.));
#7526=DIRECTION('center_axis',(0.,1.22464679914735E-16,-1.));
#7527=DIRECTION('ref_axis',(0.919145030018057,-0.39391929857917,-4.82412008127351E-17));
#7528=DIRECTION('center_axis',(0.,1.22464679914735E-16,-1.));
#7529=DIRECTION('ref_axis',(-0.887564039861159,0.460684355220946,5.64175621038594E-17));
#7530=DIRECTION('center_axis',(0.,1.22464679914735E-16,-1.));
#7531=DIRECTION('ref_axis',(1.,0.,0.));
#7532=DIRECTION('',(0.,-1.22464679914735E-16,1.));
#7533=DIRECTION('axis',(0.,0.,1.));
#7534=DIRECTION('refdir',(1.,0.,0.));
#7535=DIRECTION('center_axis',(2.22044604925031E-16,-1.,-1.22464679914735E-16));
#7536=DIRECTION('ref_axis',(-1.,-2.22044604925031E-16,-2.71926214689378E-32));
#7537=DIRECTION('center_axis',(-2.22044604925031E-16,1.,1.22464679914735E-16));
#7538=DIRECTION('ref_axis',(-1.,-2.22044604925031E-16,-2.71926214689378E-32));
#7539=DIRECTION('',(0.70710678118655,-0.707106781186545,4.95239128556718E-31));
#7540=DIRECTION('center_axis',(2.22044604925031E-16,-1.,-1.22464679914735E-16));
#7541=DIRECTION('ref_axis',(-1.,-2.22044604925031E-16,-2.71926214689378E-32));
#7542=DIRECTION('center_axis',(2.22044604925031E-16,-1.,-1.22464679914735E-16));
#7543=DIRECTION('ref_axis',(-1.,-2.22044604925031E-16,-2.71926214689378E-32));
#7544=DIRECTION('',(2.22044604925031E-16,-1.,-1.22464679914735E-16));
#7545=DIRECTION('center_axis',(-2.22044604925031E-16,1.,1.22464679914735E-16));
#7546=DIRECTION('ref_axis',(-1.,-2.22044604925031E-16,-2.71926214689378E-32));
#7547=DIRECTION('center_axis',(2.22044604925031E-16,-1.,-1.22464679914735E-16));
#7548=DIRECTION('ref_axis',(0.,-1.22464679914735E-16,1.));
#7549=DIRECTION('center_axis',(-2.22044604925031E-16,1.,1.22464679914735E-16));
#7550=DIRECTION('ref_axis',(-1.,-2.22044604925031E-16,-2.71926214689378E-32));
#7551=DIRECTION('',(-0.707106781186547,-0.707106781186548,-1.73191211247099E-16));
#7552=DIRECTION('center_axis',(2.22044604925031E-16,-1.,-1.22464679914735E-16));
#7553=DIRECTION('ref_axis',(-1.,-2.22044604925031E-16,-2.71926214689378E-32));
#7554=DIRECTION('center_axis',(2.22044604925031E-16,-1.,-1.22464679914735E-16));
#7555=DIRECTION('ref_axis',(0.,-1.22464679914735E-16,1.));
#7556=DIRECTION('axis',(0.,0.,1.));
#7557=DIRECTION('refdir',(1.,0.,0.));
#7558=DIRECTION('center_axis',(0.,0.,-1.));
#7559=DIRECTION('ref_axis',(1.,0.,0.));
#7560=DIRECTION('center_axis',(0.,-1.22464679914735E-16,1.));
#7561=DIRECTION('ref_axis',(0.,-1.,-1.22464679914735E-16));
#7562=DIRECTION('center_axis',(0.,1.,1.22464679914735E-16));
#7563=DIRECTION('ref_axis',(-1.,0.,0.));
#7564=DIRECTION('center_axis',(0.,1.22464679914735E-16,-1.));
#7565=DIRECTION('ref_axis',(1.,0.,0.));
#7566=DIRECTION('center_axis',(0.,-1.22464679914735E-16,1.));
#7567=DIRECTION('ref_axis',(1.,0.,0.));
#7568=DIRECTION('center_axis',(0.,1.,1.22464679914735E-16));
#7569=DIRECTION('ref_axis',(-1.,0.,0.));
#7570=DIRECTION('center_axis',(0.,1.22464679914735E-16,-1.));
#7571=DIRECTION('ref_axis',(1.,0.,0.));
#7572=DIRECTION('center_axis',(0.,1.22464679914735E-16,-1.));
#7573=DIRECTION('ref_axis',(1.,0.,0.));
#7574=DIRECTION('',(0.,-1.22464679914735E-16,1.));
#7575=DIRECTION('center_axis',(0.,-1.22464679914735E-16,1.));
#7576=DIRECTION('ref_axis',(1.,0.,0.));
#7577=DIRECTION('center_axis',(0.,-1.22464679914735E-16,1.));
#7578=DIRECTION('ref_axis',(1.,0.,0.));
#7579=DIRECTION('center_axis',(-0.5,-0.866025403784439,-1.06057523872491E-16));
#7580=DIRECTION('ref_axis',(-0.866025403784439,0.5,6.12323399573677E-17));
#7581=DIRECTION('',(-0.866025403784439,0.5,6.12323399573677E-17));
#7582=DIRECTION('',(0.,1.22464679914735E-16,-1.));
#7583=DIRECTION('',(-0.866025403784439,0.5,6.12323399573677E-17));
#7584=DIRECTION('',(0.,1.22464679914735E-16,-1.));
#7585=DIRECTION('center_axis',(0.5,-0.866025403784439,-1.06057523872491E-16));
#7586=DIRECTION('ref_axis',(-0.866025403784439,-0.5,-6.12323399573677E-17));
#7587=DIRECTION('',(-0.866025403784439,-0.5,-6.12323399573677E-17));
#7588=DIRECTION('',(0.,1.22464679914735E-16,-1.));
#7589=DIRECTION('',(-0.866025403784439,-0.5,-6.12323399573677E-17));
#7590=DIRECTION('center_axis',(1.,0.,0.));
#7591=DIRECTION('ref_axis',(0.,-1.,-1.22464679914735E-16));
#7592=DIRECTION('',(0.,-1.,-1.22464679914735E-16));
#7593=DIRECTION('',(0.,1.22464679914735E-16,-1.));
#7594=DIRECTION('',(0.,-1.,-1.22464679914735E-16));
#7595=DIRECTION('center_axis',(0.5,0.866025403784439,1.06057523872491E-16));
#7596=DIRECTION('ref_axis',(0.866025403784439,-0.5,-6.12323399573677E-17));
#7597=DIRECTION('',(0.866025403784439,-0.5,-6.12323399573677E-17));
#7598=DIRECTION('',(0.,1.22464679914735E-16,-1.));
#7599=DIRECTION('',(0.866025403784439,-0.5,-6.12323399573677E-17));
#7600=DIRECTION('center_axis',(-0.5,0.866025403784439,1.06057523872491E-16));
#7601=DIRECTION('ref_axis',(0.866025403784439,0.5,6.12323399573676E-17));
#7602=DIRECTION('',(0.866025403784439,0.5,6.12323399573676E-17));
#7603=DIRECTION('',(0.,1.22464679914735E-16,-1.));
#7604=DIRECTION('',(0.866025403784439,0.5,6.12323399573676E-17));
#7605=DIRECTION('center_axis',(-1.,6.40987562127855E-16,7.84983366253143E-32));
#7606=DIRECTION('ref_axis',(6.40987562127855E-16,1.,1.22464679914735E-16));
#7607=DIRECTION('',(6.40987562127855E-16,1.,1.22464679914735E-16));
#7608=DIRECTION('',(6.40987562127855E-16,1.,1.22464679914735E-16));
#7609=DIRECTION('center_axis',(0.,1.22464679914735E-16,-1.));
#7610=DIRECTION('ref_axis',(1.,0.,0.));
#7611=DIRECTION('center_axis',(0.,1.22464679914735E-16,-1.));
#7612=DIRECTION('ref_axis',(1.,0.,0.));
#7613=DIRECTION('center_axis',(0.,1.22464679914735E-16,-1.));
#7614=DIRECTION('ref_axis',(1.,0.,0.));
#7615=DIRECTION('',(-0.707106781186547,2.11959791839945E-32,-0.707106781186548));
#7616=DIRECTION('center_axis',(0.,-1.22464679914735E-16,1.));
#7617=DIRECTION('ref_axis',(1.,0.,0.));
#7618=DIRECTION('axis',(0.,0.,1.));
#7619=DIRECTION('refdir',(1.,0.,0.));
#7620=DIRECTION('center_axis',(2.22044604925031E-16,-1.,-1.22464679914735E-16));
#7621=DIRECTION('ref_axis',(0.,0.,-1.));
#7622=DIRECTION('center_axis',(-1.,-2.22044604925031E-16,0.));
#7623=DIRECTION('ref_axis',(0.,0.,1.));
#7624=DIRECTION('center_axis',(2.22044604925031E-16,-1.,-1.22464679914735E-16));
#7625=DIRECTION('ref_axis',(-2.71926214689378E-32,1.22464679914735E-16,
-1.));
#7626=DIRECTION('center_axis',(-1.,-2.22044604925031E-16,-2.71926214689378E-32));
#7627=DIRECTION('ref_axis',(-2.22044604925031E-16,1.,1.22464679914735E-16));
#7628=DIRECTION('center_axis',(1.,-1.00260219422232E-15,-1.22783356797248E-31));
#7629=DIRECTION('ref_axis',(1.00260219422232E-15,1.,1.22464679914735E-16));
#7630=DIRECTION('center_axis',(1.,-1.00260219422232E-15,-1.22783356797248E-31));
#7631=DIRECTION('ref_axis',(0.,1.22464679914735E-16,-1.));
#7632=DIRECTION('axis',(0.,0.,1.));
#7633=DIRECTION('refdir',(1.,0.,0.));
#7634=DIRECTION('center_axis',(-1.,0.,0.));
#7635=DIRECTION('ref_axis',(0.,0.,-1.));
#7636=DIRECTION('center_axis',(0.,1.,0.));
#7637=DIRECTION('ref_axis',(0.,0.,1.));
#7638=DIRECTION('center_axis',(1.,0.,0.));
#7639=DIRECTION('ref_axis',(0.,0.,-1.));
#7640=DIRECTION('center_axis',(0.,1.,1.22464679914735E-16));
#7641=DIRECTION('ref_axis',(1.,0.,0.));
#7642=DIRECTION('center_axis',(1.22464679914735E-15,-1.,-1.22464679914735E-16));
#7643=DIRECTION('ref_axis',(1.,1.22464679914735E-15,1.49975978266186E-31));
#7644=DIRECTION('center_axis',(1.22464679914735E-15,-1.,-1.22464679914735E-16));
#7645=DIRECTION('ref_axis',(0.,1.22464679914735E-16,-1.));
#7646=DIRECTION('axis',(0.,0.,1.));
#7647=DIRECTION('refdir',(1.,0.,0.));
#7648=DIRECTION('center_axis',(2.22044604925031E-16,-1.,-1.22464679914735E-16));
#7649=DIRECTION('ref_axis',(-1.,-2.22044604925031E-16,-2.71926214689378E-32));
#7650=DIRECTION('center_axis',(-2.22044604925031E-16,1.,1.22464679914735E-16));
#7651=DIRECTION('ref_axis',(-1.,-2.22044604925031E-16,-2.71926214689378E-32));
#7652=DIRECTION('',(0.70710678118655,-0.707106781186545,4.95239128556718E-31));
#7653=DIRECTION('center_axis',(2.22044604925031E-16,-1.,-1.22464679914735E-16));
#7654=DIRECTION('ref_axis',(-1.,-2.22044604925031E-16,-2.71926214689378E-32));
#7655=DIRECTION('center_axis',(2.22044604925031E-16,-1.,-1.22464679914735E-16));
#7656=DIRECTION('ref_axis',(-1.,-2.22044604925031E-16,-2.71926214689378E-32));
#7657=DIRECTION('',(2.22044604925031E-16,-1.,-1.22464679914735E-16));
#7658=DIRECTION('center_axis',(-2.22044604925031E-16,1.,1.22464679914735E-16));
#7659=DIRECTION('ref_axis',(-1.,-2.22044604925031E-16,-2.71926214689378E-32));
#7660=DIRECTION('center_axis',(2.22044604925031E-16,-1.,-1.22464679914735E-16));
#7661=DIRECTION('ref_axis',(0.,-1.22464679914735E-16,1.));
#7662=DIRECTION('center_axis',(-2.22044604925031E-16,1.,1.22464679914735E-16));
#7663=DIRECTION('ref_axis',(-1.,-2.22044604925031E-16,-2.71926214689378E-32));
#7664=DIRECTION('',(-0.707106781186547,-0.707106781186548,-1.73191211247099E-16));
#7665=DIRECTION('center_axis',(2.22044604925031E-16,-1.,-1.22464679914735E-16));
#7666=DIRECTION('ref_axis',(-1.,-2.22044604925031E-16,-2.71926214689378E-32));
#7667=DIRECTION('center_axis',(2.22044604925031E-16,-1.,-1.22464679914735E-16));
#7668=DIRECTION('ref_axis',(0.,-1.22464679914735E-16,1.));
#7669=DIRECTION('axis',(0.,0.,1.));
#7670=DIRECTION('refdir',(1.,0.,0.));
#7671=DIRECTION('center_axis',(2.22044604925031E-16,-1.,-1.22464679914735E-16));
#7672=DIRECTION('ref_axis',(0.,0.,-1.));
#7673=DIRECTION('center_axis',(-1.,-2.22044604925031E-16,0.));
#7674=DIRECTION('ref_axis',(0.,0.,1.));
#7675=DIRECTION('center_axis',(2.22044604925031E-16,-1.,-1.22464679914735E-16));
#7676=DIRECTION('ref_axis',(-2.71926214689378E-32,1.22464679914735E-16,
-1.));
#7677=DIRECTION('center_axis',(-1.,-2.22044604925031E-16,-2.71926214689378E-32));
#7678=DIRECTION('ref_axis',(-2.22044604925031E-16,1.,1.22464679914735E-16));
#7679=DIRECTION('center_axis',(1.,-1.00260219422232E-15,-1.22783356797248E-31));
#7680=DIRECTION('ref_axis',(1.00260219422232E-15,1.,1.22464679914735E-16));
#7681=DIRECTION('center_axis',(1.,-1.00260219422232E-15,-1.22783356797248E-31));
#7682=DIRECTION('ref_axis',(0.,1.22464679914735E-16,-1.));
#7683=DIRECTION('axis',(0.,0.,1.));
#7684=DIRECTION('refdir',(1.,0.,0.));
#7685=DIRECTION('center_axis',(-1.,0.,0.));
#7686=DIRECTION('ref_axis',(0.,-1.,-1.22464679914735E-16));
#7687=DIRECTION('center_axis',(-1.,0.,0.));
#7688=DIRECTION('ref_axis',(0.,-1.,-1.22464679914735E-16));
#7689=DIRECTION('',(-0.707106781186546,0.70710678118655,1.73191211247099E-16));
#7690=DIRECTION('center_axis',(1.,0.,0.));
#7691=DIRECTION('ref_axis',(0.,-1.,-1.22464679914735E-16));
#7692=DIRECTION('center_axis',(1.,0.,0.));
#7693=DIRECTION('ref_axis',(0.,-1.,-1.22464679914735E-16));
#7694=DIRECTION('',(-1.,0.,0.));
#7695=DIRECTION('center_axis',(-1.,0.,0.));
#7696=DIRECTION('ref_axis',(0.,-1.,-1.22464679914735E-16));
#7697=DIRECTION('center_axis',(1.,0.,0.));
#7698=DIRECTION('ref_axis',(0.,-1.22464679914735E-16,1.));
#7699=DIRECTION('center_axis',(1.,0.,0.));
#7700=DIRECTION('ref_axis',(0.,-1.,-1.22464679914735E-16));
#7701=DIRECTION('',(-0.707106781186548,-0.707106781186548,-1.73191211247099E-16));
#7702=DIRECTION('center_axis',(1.,0.,0.));
#7703=DIRECTION('ref_axis',(0.,-1.,-1.22464679914735E-16));
#7704=DIRECTION('center_axis',(1.,0.,0.));
#7705=DIRECTION('ref_axis',(0.,-1.22464679914735E-16,1.));
#7706=DIRECTION('axis',(0.,0.,1.));
#7707=DIRECTION('refdir',(1.,0.,0.));
#7708=DIRECTION('center_axis',(0.,0.,-1.));
#7709=DIRECTION('ref_axis',(1.,0.,0.));
#7710=DIRECTION('center_axis',(0.,-1.22464679914735E-16,1.));
#7711=DIRECTION('ref_axis',(0.,-1.,-1.22464679914735E-16));
#7712=DIRECTION('center_axis',(0.,1.,1.22464679914735E-16));
#7713=DIRECTION('ref_axis',(-1.,0.,0.));
#7714=DIRECTION('center_axis',(0.,1.22464679914735E-16,-1.));
#7715=DIRECTION('ref_axis',(1.,0.,0.));
#7716=DIRECTION('center_axis',(0.,-1.22464679914735E-16,1.));
#7717=DIRECTION('ref_axis',(1.,0.,0.));
#7718=DIRECTION('center_axis',(0.,1.,1.22464679914735E-16));
#7719=DIRECTION('ref_axis',(-1.,0.,0.));
#7720=DIRECTION('center_axis',(0.,1.22464679914735E-16,-1.));
#7721=DIRECTION('ref_axis',(1.,0.,0.));
#7722=DIRECTION('center_axis',(0.,1.22464679914735E-16,-1.));
#7723=DIRECTION('ref_axis',(1.,0.,0.));
#7724=DIRECTION('',(0.,-1.22464679914735E-16,1.));
#7725=DIRECTION('center_axis',(0.,-1.22464679914735E-16,1.));
#7726=DIRECTION('ref_axis',(1.,0.,0.));
#7727=DIRECTION('center_axis',(0.,-1.22464679914735E-16,1.));
#7728=DIRECTION('ref_axis',(1.,0.,0.));
#7729=DIRECTION('center_axis',(-0.5,-0.866025403784439,-1.06057523872491E-16));
#7730=DIRECTION('ref_axis',(-0.866025403784439,0.5,6.12323399573677E-17));
#7731=DIRECTION('',(-0.866025403784439,0.5,6.12323399573677E-17));
#7732=DIRECTION('',(0.,1.22464679914735E-16,-1.));
#7733=DIRECTION('',(-0.866025403784439,0.5,6.12323399573677E-17));
#7734=DIRECTION('',(0.,1.22464679914735E-16,-1.));
#7735=DIRECTION('center_axis',(0.5,-0.866025403784439,-1.06057523872491E-16));
#7736=DIRECTION('ref_axis',(-0.866025403784439,-0.5,-6.12323399573677E-17));
#7737=DIRECTION('',(-0.866025403784439,-0.5,-6.12323399573677E-17));
#7738=DIRECTION('',(0.,1.22464679914735E-16,-1.));
#7739=DIRECTION('',(-0.866025403784439,-0.5,-6.12323399573677E-17));
#7740=DIRECTION('center_axis',(1.,0.,0.));
#7741=DIRECTION('ref_axis',(0.,-1.,-1.22464679914735E-16));
#7742=DIRECTION('',(0.,-1.,-1.22464679914735E-16));
#7743=DIRECTION('',(0.,1.22464679914735E-16,-1.));
#7744=DIRECTION('',(0.,-1.,-1.22464679914735E-16));
#7745=DIRECTION('center_axis',(0.5,0.866025403784439,1.06057523872491E-16));
#7746=DIRECTION('ref_axis',(0.866025403784439,-0.5,-6.12323399573677E-17));
#7747=DIRECTION('',(0.866025403784439,-0.5,-6.12323399573677E-17));
#7748=DIRECTION('',(0.,1.22464679914735E-16,-1.));
#7749=DIRECTION('',(0.866025403784439,-0.5,-6.12323399573677E-17));
#7750=DIRECTION('center_axis',(-0.5,0.866025403784439,1.06057523872491E-16));
#7751=DIRECTION('ref_axis',(0.866025403784439,0.5,6.12323399573676E-17));
#7752=DIRECTION('',(0.866025403784439,0.5,6.12323399573676E-17));
#7753=DIRECTION('',(0.,1.22464679914735E-16,-1.));
#7754=DIRECTION('',(0.866025403784439,0.5,6.12323399573676E-17));
#7755=DIRECTION('center_axis',(-1.,6.40987562127855E-16,7.84983366253143E-32));
#7756=DIRECTION('ref_axis',(6.40987562127855E-16,1.,1.22464679914735E-16));
#7757=DIRECTION('',(6.40987562127855E-16,1.,1.22464679914735E-16));
#7758=DIRECTION('',(6.40987562127855E-16,1.,1.22464679914735E-16));
#7759=DIRECTION('center_axis',(0.,1.22464679914735E-16,-1.));
#7760=DIRECTION('ref_axis',(1.,0.,0.));
#7761=DIRECTION('center_axis',(0.,1.22464679914735E-16,-1.));
#7762=DIRECTION('ref_axis',(1.,0.,0.));
#7763=DIRECTION('center_axis',(0.,1.22464679914735E-16,-1.));
#7764=DIRECTION('ref_axis',(1.,0.,0.));
#7765=DIRECTION('',(-0.707106781186547,2.11959791839945E-32,-0.707106781186548));
#7766=DIRECTION('center_axis',(0.,-1.22464679914735E-16,1.));
#7767=DIRECTION('ref_axis',(1.,0.,0.));
#7768=DIRECTION('',(0.,0.,1.));
#7769=DIRECTION('',(1.,0.,0.));
#7770=DIRECTION('',(0.,0.,1.));
#7771=DIRECTION('',(1.,0.,0.));
#7772=DIRECTION('',(0.,0.,1.));
#7773=DIRECTION('',(1.,0.,0.));
#7774=DIRECTION('',(0.,0.,1.));
#7775=DIRECTION('',(1.,0.,0.));
#7776=DIRECTION('',(0.,0.,1.));
#7777=DIRECTION('',(1.,0.,0.));
#7778=DIRECTION('',(0.,0.,1.));
#7779=DIRECTION('',(1.,0.,0.));
#7780=DIRECTION('',(0.,0.,1.));
#7781=DIRECTION('',(1.,0.,0.));
#7782=DIRECTION('',(0.,0.,1.));
#7783=DIRECTION('',(1.,0.,0.));
#7784=DIRECTION('',(0.,0.,1.));
#7785=DIRECTION('',(1.,0.,0.));
#7786=DIRECTION('',(0.,0.,1.));
#7787=DIRECTION('',(1.,0.,0.));
#7788=DIRECTION('',(0.,0.,1.));
#7789=DIRECTION('',(1.,0.,0.));
#7790=DIRECTION('',(0.,0.,1.));
#7791=DIRECTION('',(1.,0.,0.));
#7792=DIRECTION('',(0.,0.,1.));
#7793=DIRECTION('',(1.,0.,0.));
#7794=CARTESIAN_POINT('',(0.,0.,0.));
#7795=CARTESIAN_POINT('',(0.,0.,0.));
#7796=CARTESIAN_POINT('Origin',(-12.2859120418715,26.4797187186996,19.));
#7797=CARTESIAN_POINT('',(-12.2859120418715,26.4797187186996,19.));
#7798=CARTESIAN_POINT('',(-12.2859120418715,27.5976499618322,19.));
#7799=CARTESIAN_POINT('',(-12.2859120418715,25.4649312716304,19.));
#7800=CARTESIAN_POINT('',(-12.2859120418715,26.4797187186996,16.5));
#7801=CARTESIAN_POINT('',(-12.2859120418715,26.4797187186996,19.));
#7802=CARTESIAN_POINT('',(-12.2859120418715,27.5976499618322,16.5));
#7803=CARTESIAN_POINT('',(-12.2859120418715,26.4797187186996,16.5));
#7804=CARTESIAN_POINT('',(-12.2859120418715,27.5976499618322,19.));
#7805=CARTESIAN_POINT('Origin',(-10.8659120418715,25.1004782148047,19.));
#7806=CARTESIAN_POINT('',(-12.2859120418715,23.7212377109099,19.));
#7807=CARTESIAN_POINT('Origin',(-10.8659120418715,25.1004782148047,19.));
#7808=CARTESIAN_POINT('',(-12.2859120418715,23.7212377109099,16.5));
#7809=CARTESIAN_POINT('',(-12.2859120418715,23.7212377109099,19.));
#7810=CARTESIAN_POINT('Origin',(-10.8659120418715,25.1004782148047,16.5));
#7811=CARTESIAN_POINT('Origin',(-12.2859120418715,22.6033064677773,19.));
#7812=CARTESIAN_POINT('',(-12.2859120418715,22.6033064677773,19.));
#7813=CARTESIAN_POINT('',(-12.2859120418715,23.5267251461693,19.));
#7814=CARTESIAN_POINT('',(-12.2859120418715,22.6033064677773,16.5));
#7815=CARTESIAN_POINT('',(-12.2859120418715,22.6033064677773,19.));
#7816=CARTESIAN_POINT('',(-12.2859120418715,22.6033064677773,16.5));
#7817=CARTESIAN_POINT('Origin',(-10.8359120418715,22.6033064677773,19.));
#7818=CARTESIAN_POINT('',(-9.3859120418715,22.6033064677773,19.));
#7819=CARTESIAN_POINT('Origin',(-10.8359120418715,22.6033064677773,19.));
#7820=CARTESIAN_POINT('',(-9.3859120418715,22.6033064677773,16.5));
#7821=CARTESIAN_POINT('',(-9.3859120418715,22.6033064677773,19.));
#7822=CARTESIAN_POINT('Origin',(-10.8359120418715,22.6033064677773,16.5));
#7823=CARTESIAN_POINT('Origin',(-9.3859120418715,23.7858283117567,19.));
#7824=CARTESIAN_POINT('',(-9.3859120418715,23.7858283117567,19.));
#7825=CARTESIAN_POINT('',(-9.3859120418715,24.117986068159,19.));
#7826=CARTESIAN_POINT('',(-9.3859120418715,23.7858283117567,16.5));
#7827=CARTESIAN_POINT('',(-9.3859120418715,23.7858283117567,19.));
#7828=CARTESIAN_POINT('',(-9.3859120418715,23.7858283117567,16.5));
#7829=CARTESIAN_POINT('Origin',(-10.8659120418715,25.1004782148047,19.));
#7830=CARTESIAN_POINT('',(-9.3859120418715,26.4151281178527,19.));
#7831=CARTESIAN_POINT('Origin',(-10.8659120418715,25.1004782148047,19.));
#7832=CARTESIAN_POINT('',(-9.3859120418715,26.4151281178527,16.5));
#7833=CARTESIAN_POINT('',(-9.3859120418715,26.4151281178527,19.));
#7834=CARTESIAN_POINT('Origin',(-10.8659120418715,25.1004782148047,16.5));
#7835=CARTESIAN_POINT('Origin',(-9.3859120418715,27.5976499618322,19.));
#7836=CARTESIAN_POINT('',(-9.3859120418715,27.5976499618322,19.));
#7837=CARTESIAN_POINT('',(-9.38591204187149,26.0238968931967,19.));
#7838=CARTESIAN_POINT('',(-9.3859120418715,27.5976499618322,16.5));
#7839=CARTESIAN_POINT('',(-9.3859120418715,27.5976499618322,19.));
#7840=CARTESIAN_POINT('',(-9.3859120418715,27.5976499618322,16.5));
#7841=CARTESIAN_POINT('Origin',(-10.8359120418715,27.5976499618322,19.));
#7842=CARTESIAN_POINT('Origin',(-10.8359120418715,27.5976499618322,19.));
#7843=CARTESIAN_POINT('Origin',(-10.8359120418715,27.5976499618322,16.5));
#7844=CARTESIAN_POINT('Origin',(-6.27876228909014,17.7140879581285,19.));
#7845=CARTESIAN_POINT('',(-6.27876228909014,17.7140879581285,19.));
#7846=CARTESIAN_POINT('',(-7.39669353222272,17.7140879581285,19.));
#7847=CARTESIAN_POINT('',(-10.9854572864952,17.7140879581285,19.));
#7848=CARTESIAN_POINT('',(-6.27876228909014,17.7140879581285,16.5));
#7849=CARTESIAN_POINT('',(-6.27876228909014,17.7140879581285,19.));
#7850=CARTESIAN_POINT('',(-7.39669353222272,17.7140879581285,16.5));
#7851=CARTESIAN_POINT('',(-6.27876228909014,17.7140879581285,16.5));
#7852=CARTESIAN_POINT('',(-7.39669353222272,17.7140879581285,19.));
#7853=CARTESIAN_POINT('Origin',(-4.89952178519528,19.1340879581285,19.));
#7854=CARTESIAN_POINT('',(-3.52028128130042,17.7140879581285,19.));
#7855=CARTESIAN_POINT('Origin',(-4.89952178519528,19.1340879581285,19.));
#7856=CARTESIAN_POINT('',(-3.52028128130042,17.7140879581285,16.5));
#7857=CARTESIAN_POINT('',(-3.52028128130042,17.7140879581285,19.));
#7858=CARTESIAN_POINT('Origin',(-4.89952178519528,19.1340879581285,16.5));
#7859=CARTESIAN_POINT('Origin',(-2.40235003816785,17.7140879581285,19.));
#7860=CARTESIAN_POINT('',(-2.40235003816785,17.7140879581285,19.));
#7861=CARTESIAN_POINT('',(-9.04725116103404,17.7140879581285,19.));
#7862=CARTESIAN_POINT('',(-2.40235003816785,17.7140879581285,16.5));
#7863=CARTESIAN_POINT('',(-2.40235003816785,17.7140879581285,19.));
#7864=CARTESIAN_POINT('',(-2.40235003816785,17.7140879581285,16.5));
#7865=CARTESIAN_POINT('Origin',(-2.40235003816784,19.1640879581285,19.));
#7866=CARTESIAN_POINT('',(-2.40235003816784,20.6140879581285,19.));
#7867=CARTESIAN_POINT('Origin',(-2.40235003816784,19.1640879581285,19.));
#7868=CARTESIAN_POINT('',(-2.40235003816784,20.6140879581285,16.5));
#7869=CARTESIAN_POINT('',(-2.40235003816784,20.6140879581285,19.));
#7870=CARTESIAN_POINT('Origin',(-2.40235003816784,19.1640879581285,16.5));
#7871=CARTESIAN_POINT('Origin',(-3.58487188214727,20.6140879581285,19.));
#7872=CARTESIAN_POINT('',(-3.58487188214727,20.6140879581285,19.));
#7873=CARTESIAN_POINT('',(-9.63851208302377,20.6140879581286,19.));
#7874=CARTESIAN_POINT('',(-3.58487188214727,20.6140879581285,16.5));
#7875=CARTESIAN_POINT('',(-3.58487188214727,20.6140879581285,19.));
#7876=CARTESIAN_POINT('',(-3.58487188214727,20.6140879581285,16.5));
#7877=CARTESIAN_POINT('Origin',(-4.89952178519528,19.1340879581285,19.));
#7878=CARTESIAN_POINT('',(-6.21417168824329,20.6140879581285,19.));
#7879=CARTESIAN_POINT('Origin',(-4.89952178519528,19.1340879581285,19.));
#7880=CARTESIAN_POINT('',(-6.21417168824329,20.6140879581285,16.5));
#7881=CARTESIAN_POINT('',(-6.21417168824329,20.6140879581285,19.));
#7882=CARTESIAN_POINT('Origin',(-4.89952178519528,19.1340879581285,16.5));
#7883=CARTESIAN_POINT('Origin',(-7.39669353222272,20.6140879581285,19.));
#7884=CARTESIAN_POINT('',(-7.39669353222272,20.6140879581285,19.));
#7885=CARTESIAN_POINT('',(-11.5444229080615,20.6140879581285,19.));
#7886=CARTESIAN_POINT('',(-7.39669353222272,20.6140879581285,16.5));
#7887=CARTESIAN_POINT('',(-7.39669353222272,20.6140879581285,19.));
#7888=CARTESIAN_POINT('',(-7.39669353222272,20.6140879581285,16.5));
#7889=CARTESIAN_POINT('Origin',(-7.39669353222272,19.1640879581285,19.));
#7890=CARTESIAN_POINT('Origin',(-7.39669353222272,19.1640879581285,19.));
#7891=CARTESIAN_POINT('Origin',(-7.39669353222272,19.1640879581285,16.5));
#7892=CARTESIAN_POINT('Origin',(-17.2859120418715,27.5976499618322,19.));
#7893=CARTESIAN_POINT('',(-17.2859120418715,27.5976499618322,19.));
#7894=CARTESIAN_POINT('',(-17.2859120418715,26.4481444819436,19.));
#7895=CARTESIAN_POINT('',(-17.2859120418715,26.0238968931967,19.));
#7896=CARTESIAN_POINT('',(-17.2859120418715,27.5976499618322,16.5));
#7897=CARTESIAN_POINT('',(-17.2859120418715,27.5976499618322,19.));
#7898=CARTESIAN_POINT('',(-17.2859120418715,26.4481444819436,16.5));
#7899=CARTESIAN_POINT('',(-17.2859120418715,27.5976499618322,16.5));
#7900=CARTESIAN_POINT('',(-17.2859120418715,26.4481444819436,19.));
#7901=CARTESIAN_POINT('Origin',(-18.7359120418715,27.5976499618322,19.));
#7902=CARTESIAN_POINT('',(-20.1859120418715,27.5976499618322,19.));
#7903=CARTESIAN_POINT('Origin',(-18.7359120418715,27.5976499618322,19.));
#7904=CARTESIAN_POINT('',(-20.1859120418715,27.5976499618322,16.5));
#7905=CARTESIAN_POINT('',(-20.1859120418715,27.5976499618322,19.));
#7906=CARTESIAN_POINT('Origin',(-18.7359120418715,27.5976499618322,16.5));
#7907=CARTESIAN_POINT('Origin',(-20.1859120418715,26.4481444819436,19.));
#7908=CARTESIAN_POINT('',(-20.1859120418715,26.4481444819436,19.));
#7909=CARTESIAN_POINT('',(-20.1859120418715,25.4491441532525,19.));
#7910=CARTESIAN_POINT('',(-20.1859120418715,26.4481444819436,16.5));
#7911=CARTESIAN_POINT('',(-20.1859120418715,26.4481444819436,19.));
#7912=CARTESIAN_POINT('',(-20.1859120418715,26.4481444819436,16.5));
#7913=CARTESIAN_POINT('Origin',(-18.7359120418715,25.1004782148047,19.));
#7914=CARTESIAN_POINT('',(-20.1859120418715,23.7528119476658,19.));
#7915=CARTESIAN_POINT('Origin',(-18.7359120418715,25.1004782148047,19.));
#7916=CARTESIAN_POINT('',(-20.1859120418715,23.7528119476658,16.5));
#7917=CARTESIAN_POINT('',(-20.1859120418715,23.7528119476658,19.));
#7918=CARTESIAN_POINT('Origin',(-18.7359120418715,25.1004782148047,16.5));
#7919=CARTESIAN_POINT('Origin',(-20.1859120418715,22.6033064677773,19.));
#7920=CARTESIAN_POINT('',(-20.1859120418715,22.6033064677773,19.));
#7921=CARTESIAN_POINT('',(-20.1859120418715,23.5267251461693,19.));
#7922=CARTESIAN_POINT('',(-20.1859120418715,22.6033064677773,16.5));
#7923=CARTESIAN_POINT('',(-20.1859120418715,22.6033064677773,19.));
#7924=CARTESIAN_POINT('',(-20.1859120418715,22.6033064677773,16.5));
#7925=CARTESIAN_POINT('Origin',(-18.7359120418715,22.6033064677773,19.));
#7926=CARTESIAN_POINT('',(-17.2859120418715,22.6033064677773,19.));
#7927=CARTESIAN_POINT('Origin',(-18.7359120418715,22.6033064677773,19.));
#7928=CARTESIAN_POINT('',(-17.2859120418715,22.6033064677773,16.5));
#7929=CARTESIAN_POINT('',(-17.2859120418715,22.6033064677773,19.));
#7930=CARTESIAN_POINT('Origin',(-18.7359120418715,22.6033064677773,16.5));
#7931=CARTESIAN_POINT('Origin',(-17.2859120418715,23.7528119476658,19.));
#7932=CARTESIAN_POINT('',(-17.2859120418715,23.7528119476658,19.));
#7933=CARTESIAN_POINT('',(-17.2859120418715,24.1014778861135,19.));
#7934=CARTESIAN_POINT('',(-17.2859120418715,23.7528119476658,16.5));
#7935=CARTESIAN_POINT('',(-17.2859120418715,23.7528119476658,19.));
#7936=CARTESIAN_POINT('',(-17.2859120418715,23.7528119476658,16.5));
#7937=CARTESIAN_POINT('Origin',(-18.7359120418715,25.1004782148047,19.));
#7938=CARTESIAN_POINT('Origin',(-18.7359120418715,25.1004782148047,19.));
#7939=CARTESIAN_POINT('Origin',(-18.7359120418715,25.1004782148047,16.5));
#7940=CARTESIAN_POINT('Origin',(-3.55185551805636,12.7140879581285,19.));
#7941=CARTESIAN_POINT('',(-3.55185551805636,12.7140879581285,19.));
#7942=CARTESIAN_POINT('',(-2.40235003816785,12.7140879581285,19.));
#7943=CARTESIAN_POINT('',(-9.6220039009783,12.7140879581285,19.));
#7944=CARTESIAN_POINT('',(-3.55185551805636,12.7140879581285,16.5));
#7945=CARTESIAN_POINT('',(-3.55185551805636,12.7140879581285,19.));
#7946=CARTESIAN_POINT('',(-2.40235003816785,12.7140879581285,16.5));
#7947=CARTESIAN_POINT('',(-3.55185551805636,12.7140879581285,16.5));
#7948=CARTESIAN_POINT('',(-2.40235003816785,12.7140879581285,19.));
#7949=CARTESIAN_POINT('Origin',(-4.89952178519528,11.2640879581285,19.));
#7950=CARTESIAN_POINT('',(-6.2471880523342,12.7140879581285,19.));
#7951=CARTESIAN_POINT('Origin',(-4.89952178519528,11.2640879581285,19.));
#7952=CARTESIAN_POINT('',(-6.2471880523342,12.7140879581285,16.5));
#7953=CARTESIAN_POINT('',(-6.2471880523342,12.7140879581285,19.));
#7954=CARTESIAN_POINT('Origin',(-4.89952178519528,11.2640879581285,16.5));
#7955=CARTESIAN_POINT('Origin',(-7.39669353222271,12.7140879581285,19.));
#7956=CARTESIAN_POINT('',(-7.39669353222271,12.7140879581285,19.));
#7957=CARTESIAN_POINT('',(-11.5444229080615,12.7140879581285,19.));
#7958=CARTESIAN_POINT('',(-7.39669353222271,12.7140879581285,16.5));
#7959=CARTESIAN_POINT('',(-7.39669353222271,12.7140879581285,19.));
#7960=CARTESIAN_POINT('',(-7.39669353222271,12.7140879581285,16.5));
#7961=CARTESIAN_POINT('Origin',(-7.39669353222271,11.2640879581285,19.));
#7962=CARTESIAN_POINT('',(-7.39669353222271,9.8140879581285,19.));
#7963=CARTESIAN_POINT('Origin',(-7.39669353222271,11.2640879581285,19.));
#7964=CARTESIAN_POINT('',(-7.39669353222271,9.8140879581285,16.5));
#7965=CARTESIAN_POINT('',(-7.39669353222271,9.8140879581285,19.));
#7966=CARTESIAN_POINT('Origin',(-7.39669353222271,11.2640879581285,16.5));
#7967=CARTESIAN_POINT('Origin',(-6.2471880523342,9.8140879581285,19.));
#7968=CARTESIAN_POINT('',(-6.2471880523342,9.8140879581285,19.));
#7969=CARTESIAN_POINT('',(-10.9696701681172,9.8140879581285,19.));
#7970=CARTESIAN_POINT('',(-6.2471880523342,9.8140879581285,16.5));
#7971=CARTESIAN_POINT('',(-6.2471880523342,9.8140879581285,19.));
#7972=CARTESIAN_POINT('',(-6.2471880523342,9.8140879581285,16.5));
#7973=CARTESIAN_POINT('Origin',(-4.89952178519528,11.2640879581285,19.));
#7974=CARTESIAN_POINT('',(-3.55185551805636,9.8140879581285,19.));
#7975=CARTESIAN_POINT('Origin',(-4.89952178519528,11.2640879581285,19.));
#7976=CARTESIAN_POINT('',(-3.55185551805636,9.8140879581285,16.5));
#7977=CARTESIAN_POINT('',(-3.55185551805636,9.8140879581285,19.));
#7978=CARTESIAN_POINT('Origin',(-4.89952178519528,11.2640879581285,16.5));
#7979=CARTESIAN_POINT('Origin',(-2.40235003816785,9.8140879581285,19.));
#7980=CARTESIAN_POINT('',(-2.40235003816785,9.8140879581285,19.));
#7981=CARTESIAN_POINT('',(-9.04725116103404,9.8140879581285,19.));
#7982=CARTESIAN_POINT('',(-2.40235003816785,9.8140879581285,16.5));
#7983=CARTESIAN_POINT('',(-2.40235003816785,9.8140879581285,19.));
#7984=CARTESIAN_POINT('',(-2.40235003816785,9.8140879581285,16.5));
#7985=CARTESIAN_POINT('Origin',(-2.40235003816785,11.2640879581285,19.));
#7986=CARTESIAN_POINT('Origin',(-2.40235003816785,11.2640879581285,19.));
#7987=CARTESIAN_POINT('Origin',(-2.40235003816785,11.2640879581285,16.5));
#7988=CARTESIAN_POINT('Origin',(-10.8659120418715,25.1004782148047,19.));
#7989=CARTESIAN_POINT('',(-12.6454838055578,25.1004782148047,8.6));
#7990=CARTESIAN_POINT('Origin',(-10.8659120418715,25.1004782148047,8.6));
#7991=CARTESIAN_POINT('',(-12.6454838055578,25.1004782148047,16.5));
#7992=CARTESIAN_POINT('',(-12.6454838055578,25.1004782148047,19.));
#7993=CARTESIAN_POINT('Origin',(-10.8659120418715,25.1004782148047,16.5));
#7994=CARTESIAN_POINT('Origin',(-4.89952178519528,11.2640879581285,19.));
#7995=CARTESIAN_POINT('',(-4.89952178519528,9.48451619444218,8.6));
#7996=CARTESIAN_POINT('Origin',(-4.89952178519528,11.2640879581285,8.6));
#7997=CARTESIAN_POINT('',(-4.89952178519528,9.48451619444219,16.5));
#7998=CARTESIAN_POINT('',(-4.89952178519528,9.48451619444219,19.));
#7999=CARTESIAN_POINT('Origin',(-4.89952178519528,11.2640879581285,16.5));
#8000=CARTESIAN_POINT('Origin',(-15.0254707357525,14.9637210836027,8.85));
#8001=CARTESIAN_POINT('',(-11.0997123508774,18.9002876491226,9.1));
#8002=CARTESIAN_POINT('',(-10.7461586545955,19.2538413470203,8.6));
#8003=CARTESIAN_POINT('Ctrl Pts',(-11.0997123508774,18.9002876491226,9.1));
#8004=CARTESIAN_POINT('Ctrl Pts',(-11.0702528871568,18.9297537969895,9.05833333333333));
#8005=CARTESIAN_POINT('Ctrl Pts',(-11.0407925873132,18.9592191099766,9.01666666666666));
#8006=CARTESIAN_POINT('Ctrl Pts',(-10.9818703154508,19.0181480661202,8.93333333333333));
#8007=CARTESIAN_POINT('Ctrl Pts',(-10.952408343432,19.0476117092766,8.89166666666666));
#8008=CARTESIAN_POINT('Ctrl Pts',(-10.8934827272903,19.1065373256877,8.80833333333333));
#8009=CARTESIAN_POINT('Ctrl Pts',(-10.8640190831674,19.1359992989424,8.76666666666667));
#8010=CARTESIAN_POINT('Ctrl Pts',(-10.8050901228885,19.1949215754788,8.68333333333333));
#8011=CARTESIAN_POINT('Ctrl Pts',(-10.7756248067326,19.2243818787606,8.64166666666666));
#8012=CARTESIAN_POINT('Ctrl Pts',(-10.7461586545955,19.2538413470203,8.6));
#8013=CARTESIAN_POINT('',(-8.96603335068975,14.9343554740278,8.6));
#8014=CARTESIAN_POINT('Origin',(-15.0254707357525,14.9637210836027,8.6));
#8015=CARTESIAN_POINT('',(-9.46602747923395,14.9367785756188,9.1));
#8016=CARTESIAN_POINT('',(-8.96603335068975,14.9343554740278,8.6));
#8017=CARTESIAN_POINT('Origin',(-15.0254707357525,14.9637210836027,9.1));
#8018=CARTESIAN_POINT('Origin',(90.5327982296072,14.4521582574094,8.85));
#8019=CARTESIAN_POINT('',(-8.96720177039285,14.4521582574094,8.6));
#8020=CARTESIAN_POINT('',(-9.46720177039287,14.4521582574094,9.1));
#8021=CARTESIAN_POINT('',(-8.96720177039285,14.4521582574094,8.6));
#8022=CARTESIAN_POINT('Origin',(90.5327982296072,14.4521582574094,9.1));
#8023=CARTESIAN_POINT('Origin',(90.5327982296072,14.4521582574094,8.6));
#8024=CARTESIAN_POINT('Origin',(-9.21720177039288,19.6482354995058,8.85));
#8025=CARTESIAN_POINT('',(-8.96720177039288,9.34727392485797,8.6));
#8026=CARTESIAN_POINT('',(-9.46720177039288,9.34727392485797,9.1));
#8027=CARTESIAN_POINT('',(-8.96720177039288,9.34727392485797,8.6));
#8028=CARTESIAN_POINT('',(-9.46720177039288,19.6482354995058,9.1));
#8029=CARTESIAN_POINT('',(-8.96720177039288,19.6482354995058,8.6));
#8030=CARTESIAN_POINT('Origin',(-7.9672017703919,9.34727392485799,8.85));
#8031=CARTESIAN_POINT('',(-8.96519438024848,9.28394343714784,8.6));
#8032=CARTESIAN_POINT('',(-9.46419068517628,9.2522781932928,9.1));
#8033=CARTESIAN_POINT('',(-8.96519438024848,9.28394343714784,8.6));
#8034=CARTESIAN_POINT('Origin',(-7.9672017703919,9.34727392485799,9.1));
#8035=CARTESIAN_POINT('Origin',(-7.9672017703919,9.34727392485799,8.6));
#8036=CARTESIAN_POINT('Origin',(-9.70746000988541,17.0333802514339,8.85));
#8037=CARTESIAN_POINT('',(-8.5966084889616,3.47558779515293,8.6));
#8038=CARTESIAN_POINT('',(-9.0956047938894,3.44392255129787,9.1));
#8039=CARTESIAN_POINT('',(-8.5966084889616,3.47558779515293,8.6));
#8040=CARTESIAN_POINT('',(-9.95695816234931,17.0175476295063,9.1));
#8041=CARTESIAN_POINT('',(-9.45796185742151,17.0492128733614,8.6));
#8042=CARTESIAN_POINT('Origin',(-8.09761218403378,3.50725303900799,8.85));
#8043=CARTESIAN_POINT('',(-8.44775642389183,3.15032305806741,8.6));
#8044=CARTESIAN_POINT('',(-8.79790066374987,2.79339307712684,9.1));
#8045=CARTESIAN_POINT('',(-8.44775642389183,3.15032305806741,8.6));
#8046=CARTESIAN_POINT('Origin',(-8.09761218403378,3.50725303900799,9.1));
#8047=CARTESIAN_POINT('Origin',(-8.09761218403378,3.50725303900799,8.6));
#8048=CARTESIAN_POINT('Origin',(-15.7926606978681,10.0053816255599,8.85));
#8049=CARTESIAN_POINT('',(-6.36480204371692,1.10696857105172,8.6));
#8050=CARTESIAN_POINT('',(-6.71494628357496,0.750038590111153,9.1));
#8051=CARTESIAN_POINT('',(-6.36480204371692,1.10696857105172,8.6));
#8052=CARTESIAN_POINT('',(-15.9677328177972,9.82691663508957,9.1));
#8053=CARTESIAN_POINT('',(-15.6175885779391,10.1838466160301,8.6));
#8054=CARTESIAN_POINT('Origin',(-6.01465780385887,1.4638985519923,8.85));
#8055=CARTESIAN_POINT('',(-6.01465780385887,0.963898551992286,8.6));
#8056=CARTESIAN_POINT('',(-6.01465780385888,0.463898551992283,9.1));
#8057=CARTESIAN_POINT('',(-6.01465780385887,0.963898551992286,8.6));
#8058=CARTESIAN_POINT('Origin',(-6.01465780385887,1.4638985519923,9.1));
#8059=CARTESIAN_POINT('Origin',(-6.01465780385887,1.4638985519923,8.6));
#8060=CARTESIAN_POINT('Origin',(-10.8534050438796,0.713898551992282,8.85));
#8061=CARTESIAN_POINT('',(-3.77953774500221,0.963898551992282,8.6));
#8062=CARTESIAN_POINT('',(-3.77953774500221,0.463898551992283,9.1));
#8063=CARTESIAN_POINT('',(-3.77953774500221,0.963898551992282,8.6));
#8064=CARTESIAN_POINT('',(-10.8534050438796,0.463898551992283,9.1));
#8065=CARTESIAN_POINT('',(-10.8534050438796,0.963898551992282,8.6));
#8066=CARTESIAN_POINT('Origin',(-3.77953774500221,1.46389855199228,8.85));
#8067=CARTESIAN_POINT('',(-3.42509449740134,1.11123726374228,8.6));
#8068=CARTESIAN_POINT('',(-3.07065124980047,0.758575975492284,9.1));
#8069=CARTESIAN_POINT('',(-3.42509449740134,1.11123726374228,8.6));
#8070=CARTESIAN_POINT('Origin',(-3.77953774500221,1.46389855199228,9.1));
#8071=CARTESIAN_POINT('Origin',(-3.77953774500221,1.46389855199228,8.6));
#8072=CARTESIAN_POINT('Origin',(-0.464527910187313,3.73231552412535,8.85));
#8073=CARTESIAN_POINT('',(-1.31055213694564,3.23646417806756,8.6));
#8074=CARTESIAN_POINT('',(-0.956108889344776,2.88380288981756,9.1));
#8075=CARTESIAN_POINT('',(-1.31055213694564,3.23646417806756,8.6));
#8076=CARTESIAN_POINT('',(-0.28730628638688,3.55598488000036,9.1));
#8077=CARTESIAN_POINT('',(-0.641749533987747,3.90864616825035,8.6));
#8078=CARTESIAN_POINT('Origin',(-1.66499538454653,3.58912546631757,8.85));
#8079=CARTESIAN_POINT('',(-1.16813965229678,3.53313992058853,8.6));
#8080=CARTESIAN_POINT('',(-0.671283920047039,3.4771543748595,9.1));
#8081=CARTESIAN_POINT('',(-1.16813965229678,3.53313992058853,8.6));
#8082=CARTESIAN_POINT('Origin',(-1.66499538454653,3.58912546631757,9.1));
#8083=CARTESIAN_POINT('Origin',(-1.66499538454653,3.58912546631757,8.6));
#8084=CARTESIAN_POINT('Origin',(0.152926315598855,13.0245040201872,8.85));
#8085=CARTESIAN_POINT('',(-0.506288535500522,9.40687959739178,8.6));
#8086=CARTESIAN_POINT('',(-0.00943280325078496,9.35089405166274,9.1));
#8087=CARTESIAN_POINT('',(-0.506288535500522,9.40687959739178,8.6));
#8088=CARTESIAN_POINT('',(0.401354181723723,12.9965112473227,9.1));
#8089=CARTESIAN_POINT('',(-0.0955015505260137,13.0524967930517,8.6));
#8090=CARTESIAN_POINT('Origin',(-1.50000000000024,9.51885068884986,8.85));
#8091=CARTESIAN_POINT('',(-0.499999999999996,9.51885068884985,8.6));
#8092=CARTESIAN_POINT('',(4.4067824247818E-15,9.51885068884984,9.1));
#8093=CARTESIAN_POINT('',(-0.499999999999996,9.51885068884985,8.6));
#8094=CARTESIAN_POINT('Origin',(-1.50000000000024,9.51885068884986,9.1));
#8095=CARTESIAN_POINT('Origin',(-1.50000000000024,9.51885068884986,8.6));
#8096=CARTESIAN_POINT('Origin',(-0.249999999999997,16.9844972567056,8.85));
#8097=CARTESIAN_POINT('',(-0.499999999999998,20.4800179767447,8.6));
#8098=CARTESIAN_POINT('',(2.11386064724713E-15,20.4800179767447,9.1));
#8099=CARTESIAN_POINT('',(-0.499999999999998,20.4800179767447,8.6));
#8100=CARTESIAN_POINT('',(2.84494650060196E-15,16.9844972567056,9.1));
#8101=CARTESIAN_POINT('',(-0.499999999999997,16.9844972567056,8.6));
#8102=CARTESIAN_POINT('Origin',(-1.50000000000038,20.4800179767447,8.85));
#8103=CARTESIAN_POINT('',(-0.507428190794775,20.6016781738967,8.6));
#8104=CARTESIAN_POINT('',(-0.011142286192162,20.6625082724727,9.1));
#8105=CARTESIAN_POINT('',(-0.507428190794775,20.6016781738967,8.6));
#8106=CARTESIAN_POINT('Origin',(-1.50000000000038,20.4800179767447,9.1));
#8107=CARTESIAN_POINT('Origin',(-1.50000000000038,20.4800179767447,8.6));
#8108=CARTESIAN_POINT('Origin',(-0.604024921256996,23.4446720175285,8.85));
#8109=CARTESIAN_POINT('',(-1.11678107889193,25.5731192264483,8.6));
#8110=CARTESIAN_POINT('',(-0.620495174289325,25.6339493250243,9.1));
#8111=CARTESIAN_POINT('',(-1.11678107889193,25.5731192264483,8.6));
#8112=CARTESIAN_POINT('',(-0.355881968955691,23.4750870668165,9.1));
#8113=CARTESIAN_POINT('',(-0.8521678735583,23.4142569682405,8.6));
#8114=CARTESIAN_POINT('Origin',(-4.88927830720691,25.1107216927931,8.85));
#8115=CARTESIAN_POINT('',(-4.42688077355167,28.8832189211081,8.6));
#8116=CARTESIAN_POINT('Origin',(-4.88927830720691,25.1107216927931,8.6));
#8117=CARTESIAN_POINT('',(-4.36605067497567,29.3795048257107,9.1));
#8118=CARTESIAN_POINT('',(-4.42688077355167,28.8832189211081,8.6));
#8119=CARTESIAN_POINT('Origin',(-4.88927830720691,25.1107216927931,9.1));
#8120=CARTESIAN_POINT('Origin',(-12.1637909407195,30.0834081721396,8.85));
#8121=CARTESIAN_POINT('',(-9.39832182610329,29.4925718092052,8.6));
#8122=CARTESIAN_POINT('',(-12.1942059900075,29.8352652198383,8.6));
#8123=CARTESIAN_POINT('',(-9.33749172752729,29.9888577138078,9.1));
#8124=CARTESIAN_POINT('',(-9.39832182610329,29.4925718092052,8.6));
#8125=CARTESIAN_POINT('',(-12.1333758914315,30.3315511244409,9.1));
#8126=CARTESIAN_POINT('Origin',(-9.51998202325534,28.4999999999996,8.85));
#8127=CARTESIAN_POINT('',(-9.51998202325534,29.5,8.6));
#8128=CARTESIAN_POINT('Origin',(-9.51998202325534,28.4999999999996,8.6));
#8129=CARTESIAN_POINT('',(-9.51998202325534,30.,9.1));
#8130=CARTESIAN_POINT('',(-9.51998202325534,29.5,8.6));
#8131=CARTESIAN_POINT('Origin',(-9.51998202325534,28.4999999999996,9.1));
#8132=CARTESIAN_POINT('Origin',(-18.0866507975252,29.75,8.85));
#8133=CARTESIAN_POINT('',(-20.4811493111502,29.5,8.6));
#8134=CARTESIAN_POINT('',(-18.0866507975252,29.5,8.6));
#8135=CARTESIAN_POINT('',(-20.4811493111502,30.,9.1));
#8136=CARTESIAN_POINT('',(-20.4811493111502,29.5,8.6));
#8137=CARTESIAN_POINT('',(-18.0866507975252,30.,9.1));
#8138=CARTESIAN_POINT('Origin',(-20.4811493111501,28.4999999999997,8.85));
#8139=CARTESIAN_POINT('',(-20.5931204026082,29.4937114644995,8.6));
#8140=CARTESIAN_POINT('Origin',(-20.4811493111501,28.4999999999998,8.6));
#8141=CARTESIAN_POINT('',(-20.6491059483372,29.9905671967492,9.1));
#8142=CARTESIAN_POINT('',(-20.5931204026082,29.4937114644995,8.6));
#8143=CARTESIAN_POINT('Origin',(-20.4811493111501,28.4999999999997,9.1));
#8144=CARTESIAN_POINT('Origin',(-21.4188131730182,29.6522547488597,8.85));
#8145=CARTESIAN_POINT('',(-26.4668600794115,28.8318603477032,8.6));
#8146=CARTESIAN_POINT('',(-21.3908204001537,29.4038268827348,8.6));
#8147=CARTESIAN_POINT('',(-26.5228456251405,29.328716079953,9.1));
#8148=CARTESIAN_POINT('',(-26.4668600794115,28.8318603477032,8.6));
#8149=CARTESIAN_POINT('',(-21.4468059458827,29.9006826149846,9.1));
#8150=CARTESIAN_POINT('Origin',(-26.4108745336824,28.3350046154535,8.85));
#8151=CARTESIAN_POINT('',(-26.7635358219324,28.6894478630543,8.6));
#8152=CARTESIAN_POINT('Origin',(-26.4108745336824,28.3350046154535,8.6));
#8153=CARTESIAN_POINT('',(-27.1161971101824,29.0438911106552,9.1));
#8154=CARTESIAN_POINT('',(-26.7635358219324,28.6894478630543,8.6));
#8155=CARTESIAN_POINT('Origin',(-26.4108745336824,28.3350046154535,9.1));
#8156=CARTESIAN_POINT('Origin',(-26.2804962944917,29.5227246824664,8.85));
#8157=CARTESIAN_POINT('',(-28.8887627362577,26.5749055025987,8.6));
#8158=CARTESIAN_POINT('',(-26.1041656503667,29.345503058666,8.6));
#8159=CARTESIAN_POINT('',(-29.2414240245077,26.9293487501995,9.1));
#8160=CARTESIAN_POINT('',(-28.8887627362577,26.5749055025987,8.6));
#8161=CARTESIAN_POINT('',(-26.4568269386167,29.6999463062668,9.1));
#8162=CARTESIAN_POINT('Origin',(-28.5361014480077,26.2204622549978,8.85));
#8163=CARTESIAN_POINT('',(-29.0361014480077,26.2204622549978,8.6));
#8164=CARTESIAN_POINT('Origin',(-28.5361014480077,26.2204622549978,8.6));
#8165=CARTESIAN_POINT('',(-29.5361014480077,26.2204622549978,9.1));
#8166=CARTESIAN_POINT('',(-29.0361014480077,26.2204622549978,8.6));
#8167=CARTESIAN_POINT('Origin',(-28.5361014480077,26.2204622549978,9.1));
#8168=CARTESIAN_POINT('Origin',(-29.2861014480077,24.2177430103512,8.85));
#8169=CARTESIAN_POINT('',(-29.0361014480077,23.9853421961411,8.6));
#8170=CARTESIAN_POINT('',(-29.0361014480077,24.2177430103512,8.6));
#8171=CARTESIAN_POINT('',(-29.5361014480077,23.9853421961411,9.1));
#8172=CARTESIAN_POINT('',(-29.0361014480077,23.9853421961411,8.6));
#8173=CARTESIAN_POINT('',(-29.5361014480077,24.2177430103512,9.1));
#8174=CARTESIAN_POINT('Origin',(-28.5361014480077,23.9853421961411,8.85));
#8175=CARTESIAN_POINT('',(-28.8930314289483,23.6351979562831,8.6));
#8176=CARTESIAN_POINT('Origin',(-28.5361014480077,23.9853421961411,8.6));
#8177=CARTESIAN_POINT('',(-29.2499614098888,23.285053716425,9.1));
#8178=CARTESIAN_POINT('',(-28.8930314289483,23.6351979562831,8.6));
#8179=CARTESIAN_POINT('Origin',(-28.5361014480077,23.9853421961411,9.1));
#8180=CARTESIAN_POINT('Origin',(-25.0166364478165,19.3266833071628,8.85));
#8181=CARTESIAN_POINT('',(-26.8496769419326,21.5522435761082,8.6));
#8182=CARTESIAN_POINT('',(-24.8381714573462,19.5017554270918,8.6));
#8183=CARTESIAN_POINT('',(-27.2066069228731,21.2020993362501,9.1));
#8184=CARTESIAN_POINT('',(-26.8496769419326,21.5522435761082,8.6));
#8185=CARTESIAN_POINT('',(-25.1951014382868,19.1516111872338,9.1));
#8186=CARTESIAN_POINT('Origin',(-26.492746960992,21.9023878159662,8.85));
#8187=CARTESIAN_POINT('',(-26.5244122048471,21.4033915110384,8.6));
#8188=CARTESIAN_POINT('Origin',(-26.492746960992,21.9023878159662,8.6));
#8189=CARTESIAN_POINT('',(-26.5560774487021,20.9043952061106,9.1));
#8190=CARTESIAN_POINT('',(-26.5244122048471,21.4033915110384,8.6));
#8191=CARTESIAN_POINT('Origin',(-26.492746960992,21.9023878159662,9.1));
#8192=CARTESIAN_POINT('Origin',(-18.337942281882,20.6333926901486,8.85));
#8193=CARTESIAN_POINT('',(-20.7160565628521,21.0348056197515,8.6));
#8194=CARTESIAN_POINT('',(-18.3221096599545,20.8828908426125,8.6));
#8195=CARTESIAN_POINT('',(-20.7477218067072,20.5358093148237,9.1));
#8196=CARTESIAN_POINT('',(-20.7160565628521,21.0348056197515,8.6));
#8197=CARTESIAN_POINT('',(-18.3537749038095,20.3838945376847,9.1));
#8198=CARTESIAN_POINT('Origin',(-20.652726075142,22.0327982296081,8.85));
#8199=CARTESIAN_POINT('',(-20.652726075142,21.0327982296071,8.6));
#8200=CARTESIAN_POINT('Origin',(-20.652726075142,22.0327982296081,8.6));
#8201=CARTESIAN_POINT('',(-20.652726075142,20.5327982296071,9.1));
#8202=CARTESIAN_POINT('',(-20.652726075142,21.0327982296071,8.6));
#8203=CARTESIAN_POINT('Origin',(-20.652726075142,22.0327982296081,9.1));
#8204=CARTESIAN_POINT('Origin',(-15.4229125547249,20.7827982296071,8.85));
#8205=CARTESIAN_POINT('',(-15.5478417425962,21.0327982296071,8.6));
#8206=CARTESIAN_POINT('',(-15.4229125547249,21.0327982296071,8.6));
#8207=CARTESIAN_POINT('',(-15.5478417425962,20.5327982296071,9.1));
#8208=CARTESIAN_POINT('',(-15.5478417425962,21.0327982296071,8.6));
#8209=CARTESIAN_POINT('',(-15.4229125547249,20.5327982296071,9.1));
#8210=CARTESIAN_POINT('Origin',(-15.5478417425962,120.532798229607,8.85000000000001));
#8211=CARTESIAN_POINT('',(-15.0656445259725,21.0339666493103,8.6));
#8212=CARTESIAN_POINT('',(-15.0632214243815,20.533972520766,9.1));
#8213=CARTESIAN_POINT('',(-15.0656445259725,21.0339666493103,8.6));
#8214=CARTESIAN_POINT('Origin',(-15.5478417425962,120.532798229607,9.10000000000001));
#8215=CARTESIAN_POINT('Origin',(-15.5478417425962,120.532798229607,8.60000000000001));
#8216=CARTESIAN_POINT('Origin',(-15.0362789163973,14.9745292642475,8.85));
#8217=CARTESIAN_POINT('Origin',(-15.0362789163973,14.9745292642475,9.1));
#8218=CARTESIAN_POINT('Origin',(-15.0362789163973,14.9745292642475,8.6));
#8219=CARTESIAN_POINT('Origin',(-9.33749172752729,29.9888577138078,19.));
#8220=CARTESIAN_POINT('',(-9.33749172752729,29.9888577138078,18.5));
#8221=CARTESIAN_POINT('',(-9.33749172752729,29.9888577138078,19.));
#8222=CARTESIAN_POINT('',(-4.36605067497567,29.3795048257107,18.5));
#8223=CARTESIAN_POINT('',(-12.1333758914315,30.3315511244409,18.5));
#8224=CARTESIAN_POINT('',(-4.36605067497567,29.3795048257107,19.));
#8225=CARTESIAN_POINT('Origin',(-9.51998202325534,28.4999999999996,19.));
#8226=CARTESIAN_POINT('',(-9.51998202325534,30.,18.5));
#8227=CARTESIAN_POINT('',(-9.51998202325534,30.,19.));
#8228=CARTESIAN_POINT('Origin',(-9.51998202325534,28.4999999999996,18.5));
#8229=CARTESIAN_POINT('Origin',(-20.4811493111501,30.,19.));
#8230=CARTESIAN_POINT('',(-20.4811493111502,30.,18.5));
#8231=CARTESIAN_POINT('',(-20.4811493111502,30.,19.));
#8232=CARTESIAN_POINT('',(-18.0866507975252,30.,18.5));
#8233=CARTESIAN_POINT('Origin',(-20.4811493111501,28.4999999999997,19.));
#8234=CARTESIAN_POINT('',(-20.6491059483372,29.9905671967492,18.5));
#8235=CARTESIAN_POINT('',(-20.6491059483372,29.9905671967492,19.));
#8236=CARTESIAN_POINT('Origin',(-20.4811493111501,28.4999999999997,18.5));
#8237=CARTESIAN_POINT('Origin',(-26.5228456251405,29.328716079953,19.));
#8238=CARTESIAN_POINT('',(-26.5228456251405,29.328716079953,18.5));
#8239=CARTESIAN_POINT('',(-26.5228456251405,29.328716079953,19.));
#8240=CARTESIAN_POINT('',(-21.4468059458827,29.9006826149846,18.5));
#8241=CARTESIAN_POINT('Origin',(-26.4108745336824,28.3350046154535,19.));
#8242=CARTESIAN_POINT('',(-27.1161971101824,29.0438911106552,18.5));
#8243=CARTESIAN_POINT('',(-27.1161971101824,29.0438911106552,19.));
#8244=CARTESIAN_POINT('Origin',(-26.4108745336824,28.3350046154535,18.5));
#8245=CARTESIAN_POINT('Origin',(-29.2414240245077,26.9293487501995,19.));
#8246=CARTESIAN_POINT('',(-29.2414240245077,26.9293487501995,18.5));
#8247=CARTESIAN_POINT('',(-29.2414240245077,26.9293487501995,19.));
#8248=CARTESIAN_POINT('',(-26.4568269386167,29.6999463062668,18.5));
#8249=CARTESIAN_POINT('Origin',(-28.5361014480077,26.2204622549978,19.));
#8250=CARTESIAN_POINT('',(-29.5361014480077,26.2204622549978,18.5));
#8251=CARTESIAN_POINT('',(-29.5361014480077,26.2204622549978,19.));
#8252=CARTESIAN_POINT('Origin',(-28.5361014480077,26.2204622549978,18.5));
#8253=CARTESIAN_POINT('Origin',(-29.5361014480077,23.9853421961411,19.));
#8254=CARTESIAN_POINT('',(-29.5361014480077,23.9853421961411,18.5));
#8255=CARTESIAN_POINT('',(-29.5361014480077,23.9853421961411,19.));
#8256=CARTESIAN_POINT('',(-29.5361014480077,24.2177430103512,18.5));
#8257=CARTESIAN_POINT('Origin',(-28.5361014480077,23.9853421961411,19.));
#8258=CARTESIAN_POINT('',(-29.2499614098888,23.285053716425,18.5));
#8259=CARTESIAN_POINT('',(-29.2499614098888,23.285053716425,19.));
#8260=CARTESIAN_POINT('Origin',(-28.5361014480077,23.9853421961411,18.5));
#8261=CARTESIAN_POINT('Origin',(-27.2066069228731,21.2020993362501,19.));
#8262=CARTESIAN_POINT('',(-27.2066069228731,21.2020993362501,18.5));
#8263=CARTESIAN_POINT('',(-27.2066069228731,21.2020993362501,19.));
#8264=CARTESIAN_POINT('',(-25.1951014382868,19.1516111872338,18.5));
#8265=CARTESIAN_POINT('Origin',(-26.492746960992,21.9023878159662,19.));
#8266=CARTESIAN_POINT('',(-26.5560774487021,20.9043952061106,18.5));
#8267=CARTESIAN_POINT('',(-26.5560774487021,20.9043952061106,19.));
#8268=CARTESIAN_POINT('Origin',(-26.492746960992,21.9023878159662,18.5));
#8269=CARTESIAN_POINT('Origin',(-20.7477218067072,20.5358093148237,19.));
#8270=CARTESIAN_POINT('',(-20.7477218067072,20.5358093148237,18.5));
#8271=CARTESIAN_POINT('',(-20.7477218067072,20.5358093148237,19.));
#8272=CARTESIAN_POINT('',(-18.3537749038095,20.3838945376847,18.5));
#8273=CARTESIAN_POINT('Origin',(-20.652726075142,22.0327982296081,19.));
#8274=CARTESIAN_POINT('',(-20.652726075142,20.5327982296071,18.5));
#8275=CARTESIAN_POINT('',(-20.652726075142,20.5327982296071,19.));
#8276=CARTESIAN_POINT('Origin',(-20.652726075142,22.0327982296081,18.5));
#8277=CARTESIAN_POINT('Origin',(-15.1536728255497,20.5327982296071,19.));
#8278=CARTESIAN_POINT('',(-15.5478417425962,20.5327982296071,18.5));
#8279=CARTESIAN_POINT('',(-15.5478417425962,20.5327982296071,19.));
#8280=CARTESIAN_POINT('',(-15.4229125547249,20.5327982296071,18.5));
#8281=CARTESIAN_POINT('Origin',(-15.5478417425962,120.532798229607,19.));
#8282=CARTESIAN_POINT('',(-15.0632214243815,20.533972520766,18.5));
#8283=CARTESIAN_POINT('',(-15.0632214243815,20.533972520766,19.));
#8284=CARTESIAN_POINT('Origin',(-15.5478417425962,120.532798229607,18.5));
#8285=CARTESIAN_POINT('Origin',(-15.0362789163973,14.9745292642475,19.));
#8286=CARTESIAN_POINT('',(-11.0997123508774,18.9002876491226,18.5));
#8287=CARTESIAN_POINT('',(-11.0997123508774,18.9002876491226,19.));
#8288=CARTESIAN_POINT('Origin',(-15.0362789163973,14.9745292642475,18.5));
#8289=CARTESIAN_POINT('Origin',(-15.0254707357525,14.9637210836027,19.));
#8290=CARTESIAN_POINT('',(-9.46602747923395,14.9367785756188,18.5));
#8291=CARTESIAN_POINT('',(-9.46602747923395,14.9367785756188,19.));
#8292=CARTESIAN_POINT('Origin',(-15.0254707357525,14.9637210836027,18.5));
#8293=CARTESIAN_POINT('Origin',(-15.6921522839002,24.4501438245613,8.6));
#8294=CARTESIAN_POINT('',(-4.88927830720691,1.65310616413992,8.6));
#8295=CARTESIAN_POINT('Origin',(-4.88927830720691,5.31072169279307,8.6));
#8296=CARTESIAN_POINT('',(-28.3468938358601,25.1107216927931,8.6));
#8297=CARTESIAN_POINT('Origin',(-24.6892783072069,25.1107216927931,8.6));
#8298=CARTESIAN_POINT('',(-4.89952178519528,17.3545161944422,8.6));
#8299=CARTESIAN_POINT('Origin',(-4.89952178519528,19.1340879581285,8.6));
#8300=CARTESIAN_POINT('',(-20.5154838055578,25.1004782148047,8.6));
#8301=CARTESIAN_POINT('Origin',(-18.7359120418715,25.1004782148047,8.6));
#8302=CARTESIAN_POINT('',(-8.54689383586007,25.1107216927931,8.6));
#8303=CARTESIAN_POINT('Origin',(-4.88927830720691,25.1107216927931,8.6));
#8304=CARTESIAN_POINT('Origin',(-15.0362789163973,14.9745292642475,18.75));
#8305=CARTESIAN_POINT('',(-10.7461586529797,19.2538413454045,19.));
#8306=CARTESIAN_POINT('Ctrl Pts',(-11.0997123508774,18.9002876491226,18.5));
#8307=CARTESIAN_POINT('Ctrl Pts',(-11.0702462030105,18.9297471128432,18.5416666666667));
#8308=CARTESIAN_POINT('Ctrl Pts',(-11.0407808900234,18.9592074126868,18.5833333333333));
#8309=CARTESIAN_POINT('Ctrl Pts',(-10.9818519338798,19.0181296845492,18.6666666666667));
#8310=CARTESIAN_POINT('Ctrl Pts',(-10.9523882907234,19.047591656568,18.7083333333333));
#8311=CARTESIAN_POINT('Ctrl Pts',(-10.8934626743122,19.1065172727097,18.7916666666667));
#8312=CARTESIAN_POINT('Ctrl Pts',(-10.8640007010576,19.1359809168326,18.8333333333333));
#8313=CARTESIAN_POINT('Ctrl Pts',(-10.8050784245212,19.1949098771114,18.9166666666667));
#8314=CARTESIAN_POINT('Ctrl Pts',(-10.7756181212394,19.2243751932674,18.9583333333333));
#8315=CARTESIAN_POINT('Ctrl Pts',(-10.7461586529797,19.2538413454045,19.));
#8316=CARTESIAN_POINT('',(-15.0656445259725,21.0339666493102,19.));
#8317=CARTESIAN_POINT('Origin',(-15.0362789163973,14.9745292642475,19.));
#8318=CARTESIAN_POINT('',(-15.0656445259725,21.0339666493102,19.));
#8319=CARTESIAN_POINT('Origin',(-15.5478417425962,120.532798229607,18.75));
#8320=CARTESIAN_POINT('',(-15.5478417425962,21.0327982296071,19.));
#8321=CARTESIAN_POINT('',(-15.5478417425962,21.0327982296071,19.));
#8322=CARTESIAN_POINT('Origin',(-15.5478417425962,120.532798229607,19.));
#8323=CARTESIAN_POINT('Origin',(-15.4229125547249,20.7827982296071,18.75));
#8324=CARTESIAN_POINT('',(-20.652726075142,21.0327982296071,19.));
#8325=CARTESIAN_POINT('',(-20.652726075142,21.0327982296071,19.));
#8326=CARTESIAN_POINT('',(-15.4229125547249,21.0327982296071,19.));
#8327=CARTESIAN_POINT('Origin',(-20.652726075142,22.0327982296081,18.75));
#8328=CARTESIAN_POINT('',(-20.7160565628522,21.0348056197515,19.));
#8329=CARTESIAN_POINT('',(-20.7160565628522,21.0348056197515,19.));
#8330=CARTESIAN_POINT('Origin',(-20.652726075142,22.0327982296081,19.));
#8331=CARTESIAN_POINT('Origin',(-18.337942281882,20.6333926901486,18.75));
#8332=CARTESIAN_POINT('',(-26.5244122048471,21.4033915110384,19.));
#8333=CARTESIAN_POINT('',(-18.3221096599545,20.8828908426125,19.));
#8334=CARTESIAN_POINT('',(-26.5244122048471,21.4033915110384,19.));
#8335=CARTESIAN_POINT('Origin',(-26.492746960992,21.9023878159662,18.75));
#8336=CARTESIAN_POINT('',(-26.8496769419326,21.5522435761082,19.));
#8337=CARTESIAN_POINT('',(-26.8496769419326,21.5522435761082,19.));
#8338=CARTESIAN_POINT('Origin',(-26.492746960992,21.9023878159662,19.));
#8339=CARTESIAN_POINT('Origin',(-25.0166364478165,19.3266833071628,18.75));
#8340=CARTESIAN_POINT('',(-28.8930314289483,23.6351979562831,19.));
#8341=CARTESIAN_POINT('',(-24.8381714573462,19.5017554270918,19.));
#8342=CARTESIAN_POINT('',(-28.8930314289483,23.6351979562831,19.));
#8343=CARTESIAN_POINT('Origin',(-28.5361014480077,23.9853421961411,18.75));
#8344=CARTESIAN_POINT('',(-29.0361014480077,23.9853421961411,19.));
#8345=CARTESIAN_POINT('',(-29.0361014480077,23.9853421961411,19.));
#8346=CARTESIAN_POINT('Origin',(-28.5361014480077,23.9853421961411,19.));
#8347=CARTESIAN_POINT('Origin',(-29.2861014480077,24.2177430103512,18.75));
#8348=CARTESIAN_POINT('',(-29.0361014480077,26.2204622549978,19.));
#8349=CARTESIAN_POINT('',(-29.0361014480077,24.2177430103512,19.));
#8350=CARTESIAN_POINT('',(-29.0361014480077,26.2204622549978,19.));
#8351=CARTESIAN_POINT('Origin',(-28.5361014480077,26.2204622549978,18.75));
#8352=CARTESIAN_POINT('',(-28.8887627362577,26.5749055025986,19.));
#8353=CARTESIAN_POINT('',(-28.8887627362577,26.5749055025986,19.));
#8354=CARTESIAN_POINT('Origin',(-28.5361014480077,26.2204622549978,19.));
#8355=CARTESIAN_POINT('Origin',(-26.2804962944917,29.5227246824664,18.75));
#8356=CARTESIAN_POINT('',(-26.7635358219324,28.6894478630543,19.));
#8357=CARTESIAN_POINT('',(-26.1041656503667,29.345503058666,19.));
#8358=CARTESIAN_POINT('',(-26.7635358219324,28.6894478630543,19.));
#8359=CARTESIAN_POINT('Origin',(-26.4108745336824,28.3350046154535,18.75));
#8360=CARTESIAN_POINT('',(-26.4668600794115,28.8318603477032,19.));
#8361=CARTESIAN_POINT('',(-26.4668600794115,28.8318603477032,19.));
#8362=CARTESIAN_POINT('Origin',(-26.4108745336824,28.3350046154535,19.));
#8363=CARTESIAN_POINT('Origin',(-21.4188131730182,29.6522547488597,18.75));
#8364=CARTESIAN_POINT('',(-20.5931204026082,29.4937114644995,19.));
#8365=CARTESIAN_POINT('',(-21.3908204001537,29.4038268827348,19.));
#8366=CARTESIAN_POINT('',(-20.5931204026082,29.4937114644995,19.));
#8367=CARTESIAN_POINT('Origin',(-20.4811493111501,28.4999999999997,18.75));
#8368=CARTESIAN_POINT('',(-20.4811493111501,29.5,19.));
#8369=CARTESIAN_POINT('',(-20.4811493111501,29.5,19.));
#8370=CARTESIAN_POINT('Origin',(-20.4811493111501,28.4999999999997,19.));
#8371=CARTESIAN_POINT('Origin',(-18.0866507975252,29.75,18.75));
#8372=CARTESIAN_POINT('',(-9.51998202325534,29.5,19.));
#8373=CARTESIAN_POINT('',(-9.51998202325534,29.5,19.));
#8374=CARTESIAN_POINT('',(-18.0866507975252,29.5,19.));
#8375=CARTESIAN_POINT('Origin',(-9.51998202325534,28.4999999999996,18.75));
#8376=CARTESIAN_POINT('',(-9.39832182610329,29.4925718092052,19.));
#8377=CARTESIAN_POINT('',(-9.39832182610329,29.4925718092052,19.));
#8378=CARTESIAN_POINT('Origin',(-9.51998202325534,28.4999999999996,19.));
#8379=CARTESIAN_POINT('Origin',(-12.1637909407195,30.0834081721396,18.75));
#8380=CARTESIAN_POINT('',(-4.42688077355167,28.8832189211081,19.));
#8381=CARTESIAN_POINT('',(-4.42688077355167,28.8832189211081,19.));
#8382=CARTESIAN_POINT('',(-12.1942059900075,29.8352652198383,19.));
#8383=CARTESIAN_POINT('Origin',(-4.88927830720691,25.1107216927931,18.75));
#8384=CARTESIAN_POINT('',(-1.11678107889194,25.5731192264483,19.));
#8385=CARTESIAN_POINT('',(-0.620495174289325,25.6339493250243,18.5));
#8386=CARTESIAN_POINT('',(-1.11678107889194,25.5731192264483,19.));
#8387=CARTESIAN_POINT('Origin',(-4.88927830720691,25.1107216927931,18.5));
#8388=CARTESIAN_POINT('Origin',(-4.88927830720691,25.1107216927931,19.));
#8389=CARTESIAN_POINT('Origin',(-0.604024921256996,23.4446720175285,18.75));
#8390=CARTESIAN_POINT('',(-0.507428190794773,20.6016781738967,19.));
#8391=CARTESIAN_POINT('',(-0.852167873558302,23.4142569682405,19.));
#8392=CARTESIAN_POINT('',(-0.011142286192162,20.6625082724727,18.5));
#8393=CARTESIAN_POINT('',(-0.507428190794773,20.6016781738967,19.));
#8394=CARTESIAN_POINT('',(-0.355881968955691,23.4750870668165,18.5));
#8395=CARTESIAN_POINT('Origin',(-1.50000000000038,20.4800179767447,18.75));
#8396=CARTESIAN_POINT('',(-0.499999999999998,20.4800179767447,19.));
#8397=CARTESIAN_POINT('Origin',(-1.50000000000038,20.4800179767447,19.));
#8398=CARTESIAN_POINT('',(2.11386064724713E-15,20.4800179767447,18.5));
#8399=CARTESIAN_POINT('',(-0.499999999999998,20.4800179767447,19.));
#8400=CARTESIAN_POINT('Origin',(-1.50000000000038,20.4800179767447,18.5));
#8401=CARTESIAN_POINT('Origin',(-0.249999999999997,16.9844972567056,18.75));
#8402=CARTESIAN_POINT('',(-0.499999999999995,9.51885068884984,19.));
#8403=CARTESIAN_POINT('',(-0.499999999999997,16.9844972567056,19.));
#8404=CARTESIAN_POINT('',(4.4067824247818E-15,9.51885068884984,18.5));
#8405=CARTESIAN_POINT('',(-0.499999999999995,9.51885068884984,19.));
#8406=CARTESIAN_POINT('',(2.84494650060196E-15,16.9844972567056,18.5));
#8407=CARTESIAN_POINT('Origin',(-1.50000000000024,9.51885068884986,18.75));
#8408=CARTESIAN_POINT('',(-0.506288535500522,9.40687959739178,19.));
#8409=CARTESIAN_POINT('Origin',(-1.50000000000024,9.51885068884986,19.));
#8410=CARTESIAN_POINT('',(-0.00943280325078496,9.35089405166275,18.5));
#8411=CARTESIAN_POINT('',(-0.506288535500522,9.40687959739178,19.));
#8412=CARTESIAN_POINT('Origin',(-1.50000000000024,9.51885068884986,18.5));
#8413=CARTESIAN_POINT('Origin',(0.152926315598855,13.0245040201872,18.75));
#8414=CARTESIAN_POINT('',(-1.16813965229678,3.53313992058853,19.));
#8415=CARTESIAN_POINT('',(-0.671283920047039,3.4771543748595,18.5));
#8416=CARTESIAN_POINT('',(-1.16813965229678,3.53313992058853,19.));
#8417=CARTESIAN_POINT('',(0.401354181723723,12.9965112473227,18.5));
#8418=CARTESIAN_POINT('',(-0.0955015505260137,13.0524967930517,19.));
#8419=CARTESIAN_POINT('Origin',(-1.66499538454653,3.58912546631758,18.75));
#8420=CARTESIAN_POINT('',(-1.31055213694565,3.23646417806756,19.));
#8421=CARTESIAN_POINT('Origin',(-1.66499538454653,3.58912546631758,19.));
#8422=CARTESIAN_POINT('',(-0.956108889344776,2.88380288981757,18.5));
#8423=CARTESIAN_POINT('',(-1.31055213694565,3.23646417806756,19.));
#8424=CARTESIAN_POINT('Origin',(-1.66499538454653,3.58912546631758,18.5));
#8425=CARTESIAN_POINT('Origin',(-0.464527910187313,3.73231552412536,18.75));
#8426=CARTESIAN_POINT('',(-3.42509449740134,1.11123726374228,19.));
#8427=CARTESIAN_POINT('',(-3.07065124980047,0.758575975492288,18.5));
#8428=CARTESIAN_POINT('',(-3.42509449740134,1.11123726374228,19.));
#8429=CARTESIAN_POINT('',(-0.28730628638688,3.55598488000036,18.5));
#8430=CARTESIAN_POINT('',(-0.641749533987747,3.90864616825036,19.));
#8431=CARTESIAN_POINT('Origin',(-3.77953774500221,1.46389855199228,18.75));
#8432=CARTESIAN_POINT('',(-3.77953774500221,0.96389855199229,19.));
#8433=CARTESIAN_POINT('Origin',(-3.77953774500221,1.46389855199228,19.));
#8434=CARTESIAN_POINT('',(-3.77953774500221,0.463898551992288,18.5));
#8435=CARTESIAN_POINT('',(-3.77953774500221,0.96389855199229,19.));
#8436=CARTESIAN_POINT('Origin',(-3.77953774500221,1.46389855199228,18.5));
#8437=CARTESIAN_POINT('Origin',(-10.8534050438796,0.713898551992287,18.75));
#8438=CARTESIAN_POINT('',(-6.01465780385888,0.963898551992286,19.));
#8439=CARTESIAN_POINT('',(-6.01465780385888,0.463898551992288,18.5));
#8440=CARTESIAN_POINT('',(-6.01465780385888,0.963898551992286,19.));
#8441=CARTESIAN_POINT('',(-10.8534050438796,0.463898551992288,18.5));
#8442=CARTESIAN_POINT('',(-10.8534050438796,0.963898551992286,19.));
#8443=CARTESIAN_POINT('Origin',(-6.01465780385887,1.4638985519923,18.75));
#8444=CARTESIAN_POINT('',(-6.36480204371692,1.10696857105173,19.));
#8445=CARTESIAN_POINT('Origin',(-6.01465780385887,1.4638985519923,19.));
#8446=CARTESIAN_POINT('',(-6.71494628357496,0.750038590111157,18.5));
#8447=CARTESIAN_POINT('',(-6.36480204371692,1.10696857105173,19.));
#8448=CARTESIAN_POINT('Origin',(-6.01465780385887,1.4638985519923,18.5));
#8449=CARTESIAN_POINT('Origin',(-15.7926606978681,10.0053816255599,18.75));
#8450=CARTESIAN_POINT('',(-8.44775642389183,3.15032305806741,19.));
#8451=CARTESIAN_POINT('',(-8.79790066374987,2.79339307712685,18.5));
#8452=CARTESIAN_POINT('',(-8.44775642389183,3.15032305806741,19.));
#8453=CARTESIAN_POINT('',(-15.9677328177972,9.82691663508957,18.5));
#8454=CARTESIAN_POINT('',(-15.6175885779391,10.1838466160301,19.));
#8455=CARTESIAN_POINT('Origin',(-8.09761218403378,3.50725303900799,18.75));
#8456=CARTESIAN_POINT('',(-8.5966084889616,3.47558779515293,19.));
#8457=CARTESIAN_POINT('Origin',(-8.09761218403378,3.50725303900799,19.));
#8458=CARTESIAN_POINT('',(-9.0956047938894,3.44392255129788,18.5));
#8459=CARTESIAN_POINT('',(-8.5966084889616,3.47558779515293,19.));
#8460=CARTESIAN_POINT('Origin',(-8.09761218403378,3.50725303900799,18.5));
#8461=CARTESIAN_POINT('Origin',(-9.70746000988541,17.0333802514339,18.75));
#8462=CARTESIAN_POINT('',(-8.96519438024848,9.28394343714786,19.));
#8463=CARTESIAN_POINT('',(-9.46419068517628,9.2522781932928,18.5));
#8464=CARTESIAN_POINT('',(-8.96519438024848,9.28394343714786,19.));
#8465=CARTESIAN_POINT('',(-9.95695816234931,17.0175476295063,18.5));
#8466=CARTESIAN_POINT('',(-9.45796185742151,17.0492128733614,19.));
#8467=CARTESIAN_POINT('Origin',(-7.9672017703919,9.34727392485799,18.75));
#8468=CARTESIAN_POINT('',(-8.96720177039288,9.34727392485798,19.));
#8469=CARTESIAN_POINT('Origin',(-7.9672017703919,9.34727392485799,19.));
#8470=CARTESIAN_POINT('',(-9.46720177039288,9.34727392485798,18.5));
#8471=CARTESIAN_POINT('',(-8.96720177039288,9.34727392485798,19.));
#8472=CARTESIAN_POINT('Origin',(-7.9672017703919,9.34727392485799,18.5));
#8473=CARTESIAN_POINT('Origin',(-9.21720177039288,19.6482354995058,18.75));
#8474=CARTESIAN_POINT('',(-8.96720177039288,14.4521582574094,19.));
#8475=CARTESIAN_POINT('',(-8.96720177039288,19.6482354995058,19.));
#8476=CARTESIAN_POINT('',(-9.46720177039287,14.4521582574094,18.5));
#8477=CARTESIAN_POINT('',(-8.96720177039288,14.4521582574094,19.));
#8478=CARTESIAN_POINT('',(-9.46720177039288,19.6482354995058,18.5));
#8479=CARTESIAN_POINT('Origin',(90.5327982296072,14.4521582574094,18.75));
#8480=CARTESIAN_POINT('',(-8.96603335068974,14.9343554740278,19.));
#8481=CARTESIAN_POINT('',(-8.96603335068974,14.9343554740278,19.));
#8482=CARTESIAN_POINT('Origin',(90.5327982296072,14.4521582574094,18.5));
#8483=CARTESIAN_POINT('Origin',(90.5327982296072,14.4521582574094,19.));
#8484=CARTESIAN_POINT('Origin',(-15.0254707357525,14.9637210836027,18.75));
#8485=CARTESIAN_POINT('Origin',(-15.0254707357525,14.9637210836027,19.));
#8486=CARTESIAN_POINT('Origin',(-0.011142286192162,20.6625082724727,19.));
#8487=CARTESIAN_POINT('',(-0.620495174289325,25.6339493250243,19.));
#8488=CARTESIAN_POINT('',(-0.011142286192162,20.6625082724727,19.));
#8489=CARTESIAN_POINT('Origin',(-1.50000000000038,20.4800179767447,19.));
#8490=CARTESIAN_POINT('',(2.11386064724713E-15,20.4800179767447,19.));
#8491=CARTESIAN_POINT('Origin',(4.53905508982503E-15,9.51885068884985,19.));
#8492=CARTESIAN_POINT('',(4.4067824247818E-15,9.51885068884984,19.));
#8493=CARTESIAN_POINT('Origin',(-1.50000000000024,9.51885068884986,19.));
#8494=CARTESIAN_POINT('',(-0.00943280325078496,9.35089405166275,19.));
#8495=CARTESIAN_POINT('Origin',(-0.671283920047039,3.4771543748595,19.));
#8496=CARTESIAN_POINT('',(-0.671283920047039,3.4771543748595,19.));
#8497=CARTESIAN_POINT('Origin',(-1.66499538454653,3.58912546631758,19.));
#8498=CARTESIAN_POINT('',(-0.956108889344776,2.88380288981757,19.));
#8499=CARTESIAN_POINT('Origin',(-3.07065124980047,0.758575975492288,19.));
#8500=CARTESIAN_POINT('',(-3.07065124980047,0.758575975492288,19.));
#8501=CARTESIAN_POINT('Origin',(-3.77953774500221,1.46389855199228,19.));
#8502=CARTESIAN_POINT('',(-3.77953774500221,0.463898551992288,19.));
#8503=CARTESIAN_POINT('Origin',(-6.01465780385888,0.463898551992288,19.));
#8504=CARTESIAN_POINT('',(-6.01465780385888,0.463898551992288,19.));
#8505=CARTESIAN_POINT('Origin',(-6.01465780385887,1.4638985519923,19.));
#8506=CARTESIAN_POINT('',(-6.71494628357496,0.750038590111157,19.));
#8507=CARTESIAN_POINT('Origin',(-8.79790066374987,2.79339307712685,19.));
#8508=CARTESIAN_POINT('',(-8.79790066374987,2.79339307712685,19.));
#8509=CARTESIAN_POINT('Origin',(-8.09761218403378,3.50725303900799,19.));
#8510=CARTESIAN_POINT('',(-9.0956047938894,3.44392255129788,19.));
#8511=CARTESIAN_POINT('Origin',(-9.46419068517628,9.2522781932928,19.));
#8512=CARTESIAN_POINT('',(-9.46419068517628,9.2522781932928,19.));
#8513=CARTESIAN_POINT('Origin',(-7.9672017703919,9.34727392485799,19.));
#8514=CARTESIAN_POINT('',(-9.46720177039288,9.34727392485798,19.));
#8515=CARTESIAN_POINT('Origin',(-9.46720177039288,14.8463271744503,19.));
#8516=CARTESIAN_POINT('',(-9.46720177039287,14.4521582574094,19.));
#8517=CARTESIAN_POINT('Origin',(90.5327982296072,14.4521582574094,19.));
#8518=CARTESIAN_POINT('Origin',(-15.6921522839002,24.4501438245613,19.));
#8519=CARTESIAN_POINT('',(-27.8468938358601,25.1107216927931,19.));
#8520=CARTESIAN_POINT('Origin',(-24.6892783072069,25.1107216927931,19.));
#8521=CARTESIAN_POINT('',(-4.88927830720691,2.15310616413992,19.));
#8522=CARTESIAN_POINT('Origin',(-4.88927830720691,5.31072169279308,19.));
#8523=CARTESIAN_POINT('',(-8.04689383586007,25.1107216927931,19.));
#8524=CARTESIAN_POINT('Origin',(-4.88927830720691,25.1107216927931,19.));
#8525=CARTESIAN_POINT('Origin',(-4.89952178519528,19.1640879581285,16.5));
#8526=CARTESIAN_POINT('',(-4.89952178519528,17.3545161944422,16.5));
#8527=CARTESIAN_POINT('Origin',(-4.89952178519528,19.1340879581285,16.5));
#8528=CARTESIAN_POINT('Origin',(-10.8359120418715,25.1004782148047,16.5));
#8529=CARTESIAN_POINT('Origin',(-4.89952178519528,11.2640879581285,16.5));
#8530=CARTESIAN_POINT('Origin',(-18.7359120418715,25.1004782148047,16.5));
#8531=CARTESIAN_POINT('',(-20.5154838055578,25.1004782148047,16.5));
#8532=CARTESIAN_POINT('Origin',(-18.7359120418715,25.1004782148047,16.5));
#8533=CARTESIAN_POINT('Origin',(-4.88927830720691,5.31072169279307,8.85));
#8534=CARTESIAN_POINT('',(-4.88927830720691,2.15310616413992,9.1));
#8535=CARTESIAN_POINT('Origin',(-4.88927830720691,5.31072169279307,9.1));
#8536=CARTESIAN_POINT('',(-4.88927830720691,1.90310616413992,8.85));
#8537=CARTESIAN_POINT('Origin',(-4.88927830720691,5.31072169279308,19.));
#8538=CARTESIAN_POINT('',(-4.88927830720691,2.15310616413992,19.));
#8539=CARTESIAN_POINT('Origin',(-4.88927830720691,25.1107216927931,8.85));
#8540=CARTESIAN_POINT('',(-8.04689383586007,25.1107216927931,9.1));
#8541=CARTESIAN_POINT('Origin',(-4.88927830720691,25.1107216927931,9.1));
#8542=CARTESIAN_POINT('',(-8.29689383586007,25.1107216927931,8.85));
#8543=CARTESIAN_POINT('Origin',(-4.88927830720691,25.1107216927931,19.));
#8544=CARTESIAN_POINT('',(-8.04689383586007,25.1107216927931,19.));
#8545=CARTESIAN_POINT('Origin',(-24.6892783072069,25.1107216927931,8.85));
#8546=CARTESIAN_POINT('',(-27.8468938358601,25.1107216927931,9.1));
#8547=CARTESIAN_POINT('',(-28.0968938358601,25.1107216927931,8.85));
#8548=CARTESIAN_POINT('Origin',(-24.6892783072069,25.1107216927931,9.1));
#8549=CARTESIAN_POINT('Origin',(-24.6892783072069,25.1107216927931,19.));
#8550=CARTESIAN_POINT('',(-27.8468938358601,25.1107216927931,19.));
#8551=CARTESIAN_POINT('Origin',(-4.89952178519528,19.1340879581285,19.));
#8552=CARTESIAN_POINT('',(-4.89952178519528,17.3545161944422,19.));
#8553=CARTESIAN_POINT('Origin',(-18.7359120418715,25.1004782148047,19.));
#8554=CARTESIAN_POINT('',(-20.5154838055578,25.1004782148047,19.));
#8555=CARTESIAN_POINT('Origin',(-4.88927830720691,25.1107216927931,19.));
#8556=CARTESIAN_POINT('',(0.,0.,0.));
#8557=CARTESIAN_POINT('Origin',(-2.24952178519528,11.2640879581285,17.6));
#8558=CARTESIAN_POINT('',(-2.19952178519528,11.9140879581285,17.6));
#8559=CARTESIAN_POINT('Origin',(-2.19952178519528,11.2640879581285,17.6));
#8560=CARTESIAN_POINT('',(-2.29952178519528,12.0140879581285,17.6));
#8561=CARTESIAN_POINT('',(-2.24952178519528,11.9640879581285,17.6));
#8562=CARTESIAN_POINT('Origin',(-2.29952178519528,11.2640879581285,17.6));
#8563=CARTESIAN_POINT('Origin',(-7.59952178519528,11.2640879581285,17.6));
#8564=CARTESIAN_POINT('',(-7.49952178519528,12.0140879581285,17.6));
#8565=CARTESIAN_POINT('',(-7.59952178519528,12.0140879581285,17.6));
#8566=CARTESIAN_POINT('Origin',(-7.49952178519528,11.2640879581285,17.6));
#8567=CARTESIAN_POINT('Origin',(-2.19952178519528,11.2640879581285,17.6));
#8568=CARTESIAN_POINT('Origin',(-7.54952178519528,11.2640879581285,17.6));
#8569=CARTESIAN_POINT('',(-7.59952178519528,11.9140879581285,17.6));
#8570=CARTESIAN_POINT('',(-7.54952178519528,11.9640879581285,17.6));
#8571=CARTESIAN_POINT('Origin',(-7.59952178519528,11.2640879581285,17.6));
#8572=CARTESIAN_POINT('Origin',(-7.59952178519528,11.2640879581285,17.6));
#8573=CARTESIAN_POINT('',(0.,0.,0.));
#8574=CARTESIAN_POINT('Origin',(-3.64952178519528,11.2640879581285,17.6));
#8575=CARTESIAN_POINT('',(-3.64952178519528,11.2640879581285,18.35));
#8576=CARTESIAN_POINT('Origin',(-3.64952178519528,11.2640879581285,18.6));
#8577=CARTESIAN_POINT('Origin',(-3.64952178519528,11.2640879581285,17.6));
#8578=CARTESIAN_POINT('',(-3.39952178519528,11.2640879581285,16.6));
#8579=CARTESIAN_POINT('',(-3.89952178519528,11.2640879581285,16.6));
#8580=CARTESIAN_POINT('Origin',(-3.64952178519528,11.2640879581285,16.6));
#8581=CARTESIAN_POINT('Ctrl Pts',(-3.39952178519528,11.2640879581285,16.6));
#8582=CARTESIAN_POINT('Ctrl Pts',(-3.39952178519528,11.2597806646461,16.5977092724426));
#8583=CARTESIAN_POINT('Ctrl Pts',(-3.39955324129755,11.2554410535254,16.5954788663774));
#8584=CARTESIAN_POINT('Ctrl Pts',(-3.40014364770956,11.2127459875283,16.5742560748851));
#8585=CARTESIAN_POINT('Ctrl Pts',(-3.40282286847409,11.1716935753448,16.559542959919));
#8586=CARTESIAN_POINT('Ctrl Pts',(-3.40690999909243,11.1298891387388,16.5481972195909));
#8587=CARTESIAN_POINT('Ctrl Pts',(-3.40698112962582,11.1291660315159,16.5480020646239));
#8588=CARTESIAN_POINT('Ctrl Pts',(-3.4081629902897,11.1172240770089,16.544797109728));
#8589=CARTESIAN_POINT('Ctrl Pts',(-3.409384175847,11.105936706496,16.5420298581508));
#8590=CARTESIAN_POINT('Ctrl Pts',(-3.41126371924574,11.089929722745,16.5384418503857));
#8591=CARTESIAN_POINT('Ctrl Pts',(-3.4118338437146,11.0852272650427,16.5374286265409));
#8592=CARTESIAN_POINT('Ctrl Pts',(-3.41287366194149,11.0769152925628,16.5357072275207));
#8593=CARTESIAN_POINT('Ctrl Pts',(-3.41333572893562,11.0733067646504,16.5349829852478));
#8594=CARTESIAN_POINT('Ctrl Pts',(-3.41433854491902,11.0656535215358,16.5334946079531));
#8595=CARTESIAN_POINT('Ctrl Pts',(-3.41488223353522,11.0616071709856,16.5327358435474));
#8596=CARTESIAN_POINT('Ctrl Pts',(-3.4162295106395,11.0518266202365,16.5309679692519));
#8597=CARTESIAN_POINT('Ctrl Pts',(-3.41704752686023,11.0460875459453,16.5299854641958));
#8598=CARTESIAN_POINT('Ctrl Pts',(-3.4199708406405,11.0262612081367,16.5267739133408));
#8599=CARTESIAN_POINT('Ctrl Pts',(-3.42222357481902,11.0121330333764,16.5248034466825));
#8600=CARTESIAN_POINT('Ctrl Pts',(-3.43123014519201,10.9599127812053,16.5186110231589));
#8601=CARTESIAN_POINT('Ctrl Pts',(-3.4391986219584,10.9214946617958,16.5162061142361));
#8602=CARTESIAN_POINT('Ctrl Pts',(-3.45515688387283,10.8586436195296,16.5154725363415));
#8603=CARTESIAN_POINT('Ctrl Pts',(-3.46228620261987,10.8336658536588,16.5160451884648));
#8604=CARTESIAN_POINT('Ctrl Pts',(-3.49512947595985,10.7324932763169,16.5219235534991));
#8605=CARTESIAN_POINT('Ctrl Pts',(-3.52630916660788,10.6660472824376,16.5341985199053));
#8606=CARTESIAN_POINT('Ctrl Pts',(-3.59133594943102,10.5724026680879,16.5639151059098));
#8607=CARTESIAN_POINT('Ctrl Pts',(-3.62203715988421,10.5415254901727,16.5791986989673));
#8608=CARTESIAN_POINT('Ctrl Pts',(-3.67499828617909,10.506956937443,16.605627659773));
#8609=CARTESIAN_POINT('Ctrl Pts',(-3.69704039179924,10.4980988346278,16.6166575639151));
#8610=CARTESIAN_POINT('Ctrl Pts',(-3.73479375210779,10.4922551407825,16.6350648852536));
#8611=CARTESIAN_POINT('Ctrl Pts',(-3.75139876442454,10.4929258201185,16.6429988757827));
#8612=CARTESIAN_POINT('Ctrl Pts',(-3.78199607956949,10.501731549649,16.6569651923278));
#8613=CARTESIAN_POINT('Ctrl Pts',(-3.79535203986082,10.5088054563803,16.6627780404676));
#8614=CARTESIAN_POINT('Ctrl Pts',(-3.82105390005994,10.5293269577824,16.6732083185761));
#8615=CARTESIAN_POINT('Ctrl Pts',(-3.83248647058025,10.5428683869631,16.677362768157));
#8616=CARTESIAN_POINT('Ctrl Pts',(-3.85612750484055,10.5800246546226,16.6848437491615));
#8617=CARTESIAN_POINT('Ctrl Pts',(-3.86624809413459,10.6053078595428,16.686910649375));
#8618=CARTESIAN_POINT('Ctrl Pts',(-3.88756792802042,10.6782927145015,16.6888104810606));
#8619=CARTESIAN_POINT('Ctrl Pts',(-3.89396521465656,10.7328116182588,16.6853604690573));
#8620=CARTESIAN_POINT('Ctrl Pts',(-3.90307097190431,10.9018817770723,16.6690502405298));
#8621=CARTESIAN_POINT('Ctrl Pts',(-3.89916166722153,11.1142796138527,16.6427595546923));
#8622=CARTESIAN_POINT('Ctrl Pts',(-3.89951831852135,11.258896367419,16.6015112866721));
#8623=CARTESIAN_POINT('Ctrl Pts',(-3.89952178519528,11.261493424974,16.6007604391535));
#8624=CARTESIAN_POINT('Ctrl Pts',(-3.89952178519528,11.2640879581285,16.6));
#8625=CARTESIAN_POINT('Ctrl Pts',(-3.89952178519528,11.2640879581285,16.6));
#8626=CARTESIAN_POINT('Ctrl Pts',(-3.89952178519528,11.100463340754,16.553125));
#8627=CARTESIAN_POINT('Ctrl Pts',(-3.98202611573229,10.7745871843551,16.459375));
#8628=CARTESIAN_POINT('Ctrl Pts',(-4.43258063114212,10.2697743643378,16.271875));
#8629=CARTESIAN_POINT('Ctrl Pts',(-5.34805346405984,10.1770907055197,16.0375));
#8630=CARTESIAN_POINT('Ctrl Pts',(-6.05333301021299,11.0351030238058,15.75625));
#8631=CARTESIAN_POINT('Ctrl Pts',(-5.7305291347766,12.0952484733215,15.475));
#8632=CARTESIAN_POINT('Ctrl Pts',(-4.67032720528385,12.41730825404,15.19375));
#8633=CARTESIAN_POINT('Ctrl Pts',(-3.81321563500956,11.71396418737,14.9125));
#8634=CARTESIAN_POINT('Ctrl Pts',(-3.92199706138937,10.6109219094395,14.63125));
#8635=CARTESIAN_POINT('Ctrl Pts',(-4.89949901982681,10.0883621413897,14.35));
#8636=CARTESIAN_POINT('Ctrl Pts',(-5.87710301444863,10.6109032023111,14.06875));
#8637=CARTESIAN_POINT('Ctrl Pts',(-5.98573321383868,11.7140106207574,13.7875));
#8638=CARTESIAN_POINT('Ctrl Pts',(-5.12889498447605,12.4172116991036,13.50625));
#8639=CARTESIAN_POINT('Ctrl Pts',(-4.06816558640322,12.095441826144,13.225));
#8640=CARTESIAN_POINT('Ctrl Pts',(-3.74640046021744,11.0347181280085,12.94375));
#8641=CARTESIAN_POINT('Ctrl Pts',(-4.44959545666081,10.177870497758,12.6625));
#8642=CARTESIAN_POINT('Ctrl Pts',(-5.55271322406204,10.2865183309037,12.38125));
#8643=CARTESIAN_POINT('Ctrl Pts',(-6.07523468001534,11.2640879581285,12.1));
#8644=CARTESIAN_POINT('Ctrl Pts',(-5.55271322406204,12.2416575853533,11.81875));
#8645=CARTESIAN_POINT('Ctrl Pts',(-4.44959545666081,12.3503054184991,11.5375));
#8646=CARTESIAN_POINT('Ctrl Pts',(-3.74640046021743,11.4934577882485,11.25625));
#8647=CARTESIAN_POINT('Ctrl Pts',(-4.06816558640323,10.432734090113,10.975));
#8648=CARTESIAN_POINT('Ctrl Pts',(-5.12889498447604,10.1109642171534,10.69375));
#8649=CARTESIAN_POINT('Ctrl Pts',(-5.98573321383869,10.8141652954996,10.4125));
#8650=CARTESIAN_POINT('Ctrl Pts',(-5.87710301444862,11.9172727139459,10.13125));
#8651=CARTESIAN_POINT('Ctrl Pts',(-4.89949901982682,12.4398137748673,9.85));
#8652=CARTESIAN_POINT('Ctrl Pts',(-3.92199706138938,11.9172540068175,9.56875));
#8653=CARTESIAN_POINT('Ctrl Pts',(-3.81321563500956,10.8142117288869,9.2875));
#8654=CARTESIAN_POINT('Ctrl Pts',(-4.67032720528385,10.110867662217,9.00625));
#8655=CARTESIAN_POINT('Ctrl Pts',(-5.73052913477659,10.4329274429355,8.725));
#8656=CARTESIAN_POINT('Ctrl Pts',(-6.05333301021299,11.4930728924512,8.44374999999999));
#8657=CARTESIAN_POINT('Ctrl Pts',(-5.34805346405984,12.3510852107373,8.16250000000001));
#8658=CARTESIAN_POINT('Ctrl Pts',(-4.43258063114213,12.2584015519192,7.92812499999999));
#8659=CARTESIAN_POINT('Ctrl Pts',(-3.98202611573229,11.7535887319019,7.740625));
#8660=CARTESIAN_POINT('Ctrl Pts',(-3.89952178519528,11.427712575503,7.646875));
#8661=CARTESIAN_POINT('Ctrl Pts',(-3.89952178519528,11.2640879581285,7.6));
#8662=CARTESIAN_POINT('Ctrl Pts',(-3.89952178519528,11.2640879581285,16.5439001311859));
#8663=CARTESIAN_POINT('Ctrl Pts',(-3.89952178519528,11.1005177695264,16.4970251311859));
#8664=CARTESIAN_POINT('Ctrl Pts',(-3.98203954157123,10.7745703060467,16.4032751311859));
#8665=CARTESIAN_POINT('Ctrl Pts',(-4.43255286964902,10.2698405453218,16.2157751311859));
#8666=CARTESIAN_POINT('Ctrl Pts',(-5.34806550647335,10.1770785267943,15.9814001311859));
#8667=CARTESIAN_POINT('Ctrl Pts',(-6.05330687653147,11.0351202247863,15.7001501311859));
#8668=CARTESIAN_POINT('Ctrl Pts',(-5.73052148986863,12.0952292689555,15.4189001311859));
#8669=CARTESIAN_POINT('Ctrl Pts',(-4.67032825737134,12.4172947840889,15.1376501311859));
#8670=CARTESIAN_POINT('Ctrl Pts',(-3.81323281431783,11.7139557792958,14.8564001311859));
#8671=CARTESIAN_POINT('Ctrl Pts',(-3.92201086686978,10.6109324328155,14.5751501311859));
#8672=CARTESIAN_POINT('Ctrl Pts',(-4.89949932136982,10.0883790058937,14.2939001311859));
#8673=CARTESIAN_POINT('Ctrl Pts',(-5.87708846051385,10.6109130556342,14.0126501311859));
#8674=CARTESIAN_POINT('Ctrl Pts',(-5.98571728919321,11.7140038758466,13.7314001311859));
#8675=CARTESIAN_POINT('Ctrl Pts',(-5.12889156632292,12.4171947705987,13.4501501311859));
#8676=CARTESIAN_POINT('Ctrl Pts',(-4.06817785358609,12.0954295490545,13.1689001311859));
#8677=CARTESIAN_POINT('Ctrl Pts',(-3.74641743755984,11.0347215219131,12.8876501311859));
#8678=CARTESIAN_POINT('Ctrl Pts',(-4.44960209025997,10.1778864924967,12.6064001311859));
#8679=CARTESIAN_POINT('Ctrl Pts',(-5.55270359818498,10.2865327351104,12.3251501311859));
#8680=CARTESIAN_POINT('Ctrl Pts',(-6.07521736228489,11.2640879581285,12.0439001311859));
#8681=CARTESIAN_POINT('Ctrl Pts',(-5.55270359818497,12.2416431811466,11.7626501311859));
#8682=CARTESIAN_POINT('Ctrl Pts',(-4.44960209025998,12.3502894237603,11.4814001311859));
#8683=CARTESIAN_POINT('Ctrl Pts',(-3.74641743755983,11.4934543943439,11.2001501311859));
#8684=CARTESIAN_POINT('Ctrl Pts',(-4.0681778535861,10.4327463672025,10.9189001311859));
#8685=CARTESIAN_POINT('Ctrl Pts',(-5.12889156632293,10.1109811456583,10.6376501311859));
#8686=CARTESIAN_POINT('Ctrl Pts',(-5.98571728919321,10.8141720404104,10.3564001311859));
#8687=CARTESIAN_POINT('Ctrl Pts',(-5.87708846051386,11.9172628606228,10.0751501311859));
#8688=CARTESIAN_POINT('Ctrl Pts',(-4.89949932136981,12.4397969103633,9.79390013118588));
#8689=CARTESIAN_POINT('Ctrl Pts',(-3.92201086686979,11.9172434834415,9.51265013118591));
#8690=CARTESIAN_POINT('Ctrl Pts',(-3.81323281431782,10.8142201369612,9.23140013118588));
#8691=CARTESIAN_POINT('Ctrl Pts',(-4.67032825737135,10.1108811321681,8.95015013118591));
#8692=CARTESIAN_POINT('Ctrl Pts',(-5.73052148986861,10.4329466473015,8.66890013118588));
#8693=CARTESIAN_POINT('Ctrl Pts',(-6.05330687653148,11.4930556914707,8.3876501311859));
#8694=CARTESIAN_POINT('Ctrl Pts',(-5.34806550647334,12.3510973894627,8.10640013118589));
#8695=CARTESIAN_POINT('Ctrl Pts',(-4.43255286964902,12.2583353709352,7.87202513118589));
#8696=CARTESIAN_POINT('Ctrl Pts',(-3.98203954157123,11.7536056102103,7.6845251311859));
#8697=CARTESIAN_POINT('Ctrl Pts',(-3.89952178519528,11.4276581467306,7.59077513118589));
#8698=CARTESIAN_POINT('Ctrl Pts',(-3.89952178519528,11.2640879581285,7.54390013118589));
#8699=CARTESIAN_POINT('Ctrl Pts',(-3.87336950513992,11.2640879581285,16.4693438123938));
#8700=CARTESIAN_POINT('Ctrl Pts',(-3.87336950513992,11.0961655481765,16.4224688123938));
#8701=CARTESIAN_POINT('Ctrl Pts',(-3.95802691518839,10.7617914019627,16.3287188123938));
#8702=CARTESIAN_POINT('Ctrl Pts',(-4.42037856051485,10.2437481371936,16.1412188123938));
#8703=CARTESIAN_POINT('Ctrl Pts',(-5.35977946696098,10.1486674187998,15.9068438123938));
#8704=CARTESIAN_POINT('Ctrl Pts',(-6.08351675236037,11.0291086562651,15.6255938123938));
#8705=CARTESIAN_POINT('Ctrl Pts',(-5.75226448923586,12.1169917912308,15.3443438123938));
#8706=CARTESIAN_POINT('Ctrl Pts',(-4.66433288422069,12.4474722061341,15.0630938123938));
#8707=CARTESIAN_POINT('Ctrl Pts',(-3.78480037035456,11.7257323553314,14.7818438123938));
#8708=CARTESIAN_POINT('Ctrl Pts',(-3.89642783422015,10.5938365249336,14.5005938123939));
#8709=CARTESIAN_POINT('Ctrl Pts',(-4.8994983212158,10.0576084563578,14.2193438123938));
#8710=CARTESIAN_POINT('Ctrl Pts',(-5.90267397562595,10.5938175579892,13.9380938123938));
#8711=CARTESIAN_POINT('Ctrl Pts',(-6.01414557172786,11.7257794336104,13.6568438123938));
#8712=CARTESIAN_POINT('Ctrl Pts',(-5.13489478695554,12.4473743102335,13.3755938123938));
#8713=CARTESIAN_POINT('Ctrl Pts',(-4.0464195261301,12.1171878288539,13.0943438123938));
#8714=CARTESIAN_POINT('Ctrl Pts',(-3.71623789555002,11.0287184219426,12.8130938123938));
#8715=CARTESIAN_POINT('Ctrl Pts',(-4.43782658604776,10.1494579581263,12.5318438123938));
#8716=CARTESIAN_POINT('Ctrl Pts',(-5.56979896528612,10.260947724411,12.2505938123938));
#8717=CARTESIAN_POINT('Ctrl Pts',(-6.10598818228894,11.2640879581285,11.9693438123938));
#8718=CARTESIAN_POINT('Ctrl Pts',(-5.56979896528612,12.267228191846,11.6880938123938));
#8719=CARTESIAN_POINT('Ctrl Pts',(-4.43782658604776,12.3787179581308,11.4068438123938));
#8720=CARTESIAN_POINT('Ctrl Pts',(-3.71623789555002,11.4994574943143,11.1255938123938));
#8721=CARTESIAN_POINT('Ctrl Pts',(-4.0464195261301,10.4109880874031,10.8443438123939));
#8722=CARTESIAN_POINT('Ctrl Pts',(-5.13489478695554,10.0808016060235,10.5630938123938));
#8723=CARTESIAN_POINT('Ctrl Pts',(-6.01414557172786,10.8023964826466,10.2818438123938));
#8724=CARTESIAN_POINT('Ctrl Pts',(-5.90267397562594,11.9343583582678,10.0005938123938));
#8725=CARTESIAN_POINT('Ctrl Pts',(-4.89949832121581,12.4705674598992,9.71934381239383));
#8726=CARTESIAN_POINT('Ctrl Pts',(-3.89642783422016,11.9343393913234,9.43809381239383));
#8727=CARTESIAN_POINT('Ctrl Pts',(-3.78480037035456,10.8024435609256,9.15684381239382));
#8728=CARTESIAN_POINT('Ctrl Pts',(-4.66433288422068,10.0807037101229,8.87559381239384));
#8729=CARTESIAN_POINT('Ctrl Pts',(-5.75226448923587,10.4111841250261,8.59434381239382));
#8730=CARTESIAN_POINT('Ctrl Pts',(-6.08351675236036,11.4990672599919,8.31309381239383));
#8731=CARTESIAN_POINT('Ctrl Pts',(-5.35977946696099,12.3795084974572,8.03184381239384));
#8732=CARTESIAN_POINT('Ctrl Pts',(-4.42037856051485,12.2844277790635,7.79746881239382));
#8733=CARTESIAN_POINT('Ctrl Pts',(-3.95802691518839,11.7663845142943,7.60996881239383));
#8734=CARTESIAN_POINT('Ctrl Pts',(-3.87336950513992,11.4320103680805,7.51621881239383));
#8735=CARTESIAN_POINT('Ctrl Pts',(-3.87336950513992,11.2640879581285,7.46934381239383));
#8736=CARTESIAN_POINT('Ctrl Pts',(-3.79339036013458,11.2640879581285,16.3896607060098));
#8737=CARTESIAN_POINT('Ctrl Pts',(-3.79339036013458,11.0831088802229,16.3427857060098));
#8738=CARTESIAN_POINT('Ctrl Pts',(-3.8846537686712,10.7226322800334,16.2490357060098));
#8739=CARTESIAN_POINT('Ctrl Pts',(-4.38301776128431,10.1642601287568,16.0615357060098));
#8740=CARTESIAN_POINT('Ctrl Pts',(-5.39565926012194,10.0617236200811,15.8271607060098));
#8741=CARTESIAN_POINT('Ctrl Pts',(-6.17578323657063,11.0108040827547,15.5459107060098));
#8742=CARTESIAN_POINT('Ctrl Pts',(-5.81872354841958,12.1834567527021,15.2646607060098));
#8743=CARTESIAN_POINT('Ctrl Pts',(-4.6460026754234,12.5396983825077,14.9834107060098));
#8744=CARTESIAN_POINT('Ctrl Pts',(-3.69792796710343,11.7617084542898,14.7021607060098));
#8745=CARTESIAN_POINT('Ctrl Pts',(-3.81825382373765,10.5416026416254,14.4209107060098));
#8746=CARTESIAN_POINT('Ctrl Pts',(-4.8994966660506,9.96358417175727,14.1396607060098));
#8747=CARTESIAN_POINT('Ctrl Pts',(-5.98085209435916,10.5415818105476,13.8584107060098));
#8748=CARTESIAN_POINT('Ctrl Pts',(-6.10101108821724,11.761760159582,13.5771607060098));
#8749=CARTESIAN_POINT('Ctrl Pts',(-5.15323798227467,12.5395908649936,13.2959107060098));
#8750=CARTESIAN_POINT('Ctrl Pts',(-3.97993510456335,12.183672058567,13.0146607060098));
#8751=CARTESIAN_POINT('Ctrl Pts',(-3.62402156083799,11.0103754827702,12.7334107060098));
#8752=CARTESIAN_POINT('Ctrl Pts',(-4.40184550575446,10.0625919977156,12.4521607060099));
#8753=CARTESIAN_POINT('Ctrl Pts',(-5.62203537213207,10.1827704513763,12.1709107060098));
#8754=CARTESIAN_POINT('Ctrl Pts',(-6.20001118452041,11.2640879581285,11.8896607060099));
#8755=CARTESIAN_POINT('Ctrl Pts',(-5.62203537213207,12.3454054648807,11.6084107060098));
#8756=CARTESIAN_POINT('Ctrl Pts',(-4.40184550575447,12.4655839185415,11.3271607060098));
#8757=CARTESIAN_POINT('Ctrl Pts',(-3.62402156083798,11.5178004334867,11.0459107060098));
#8758=CARTESIAN_POINT('Ctrl Pts',(-3.97993510456335,10.34450385769,10.7646607060098));
#8759=CARTESIAN_POINT('Ctrl Pts',(-5.15323798227467,9.98858505126339,10.4834107060098));
#8760=CARTESIAN_POINT('Ctrl Pts',(-6.10101108821723,10.766415756675,10.2021607060098));
#8761=CARTESIAN_POINT('Ctrl Pts',(-5.98085209435917,11.9865941057094,9.92091070600982));
#8762=CARTESIAN_POINT('Ctrl Pts',(-4.89949666605059,12.5645917444997,9.63966070600984));
#8763=CARTESIAN_POINT('Ctrl Pts',(-3.81825382373766,11.9865732746316,9.35841070600983));
#8764=CARTESIAN_POINT('Ctrl Pts',(-3.69792796710343,10.7664674619671,9.07716070600983));
#8765=CARTESIAN_POINT('Ctrl Pts',(-4.64600267542341,9.98847753374938,8.79591070600983));
#8766=CARTESIAN_POINT('Ctrl Pts',(-5.81872354841957,10.3447191635549,8.51466070600983));
#8767=CARTESIAN_POINT('Ctrl Pts',(-6.17578323657063,11.5173718335023,8.23341070600984));
#8768=CARTESIAN_POINT('Ctrl Pts',(-5.39565926012194,12.4664522961759,7.95216070600983));
#8769=CARTESIAN_POINT('Ctrl Pts',(-4.38301776128432,12.3639157875002,7.71778570600983));
#8770=CARTESIAN_POINT('Ctrl Pts',(-3.8846537686712,11.8055436362236,7.53028570600983));
#8771=CARTESIAN_POINT('Ctrl Pts',(-3.79339036013458,11.4450670360341,7.43653570600983));
#8772=CARTESIAN_POINT('Ctrl Pts',(-3.79339036013458,11.2640879581285,7.38966070600983));
#8773=CARTESIAN_POINT('Ctrl Pts',(-3.68970487524127,11.2640879581285,16.3393272852701));
#8774=CARTESIAN_POINT('Ctrl Pts',(-3.68970487524127,11.0661279362491,16.2924522852701));
#8775=CARTESIAN_POINT('Ctrl Pts',(-3.78951897521615,10.6718829447944,16.1987022852701));
#8776=CARTESIAN_POINT('Ctrl Pts',(-4.33461061966199,10.0611454603422,16.0112022852701));
#8777=CARTESIAN_POINT('Ctrl Pts',(-5.44216206725399,9.9490212390312,15.7768272852701));
#8778=CARTESIAN_POINT('Ctrl Pts',(-6.2954241293124,10.9870567873906,15.4955772852701));
#8779=CARTESIAN_POINT('Ctrl Pts',(-5.90488911793673,12.2696414836945,15.2143272852701));
#8780=CARTESIAN_POINT('Ctrl Pts',(-4.62223822570157,12.6592744106758,14.9330772852701));
#8781=CARTESIAN_POINT('Ctrl Pts',(-3.58528891191358,11.8083564753633,14.6518272852701));
#8782=CARTESIAN_POINT('Ctrl Pts',(-3.71689478093803,10.4738758167534,14.3705772852701));
#8783=CARTESIAN_POINT('Ctrl Pts',(-4.89949422003833,9.84167368441925,14.0893272852701));
#8784=CARTESIAN_POINT('Ctrl Pts',(-6.08221720835516,10.4738532361703,13.8080772852701));
#8785=CARTESIAN_POINT('Ctrl Pts',(-6.213639966101,11.8084125231395,13.5268272852701));
#8786=CARTESIAN_POINT('Ctrl Pts',(-5.17702162369123,12.6591578633091,13.2455772852701));
#8787=CARTESIAN_POINT('Ctrl Pts',(-3.89373205270486,12.2698748715692,12.9643272852701));
#8788=CARTESIAN_POINT('Ctrl Pts',(-3.50445479916688,10.9865921975682,12.6830772852701));
#8789=CARTESIAN_POINT('Ctrl Pts',(-4.35519279368454,9.94996247453771,12.4018272852701));
#8790=CARTESIAN_POINT('Ctrl Pts',(-5.68976457489842,10.0814065828331,12.1205772852701));
#8791=CARTESIAN_POINT('Ctrl Pts',(-6.32192046066284,11.2640879581285,11.8393272852701));
#8792=CARTESIAN_POINT('Ctrl Pts',(-5.68976457489842,12.4467693334238,11.5580772852701));
#8793=CARTESIAN_POINT('Ctrl Pts',(-4.35519279368455,12.5782134417193,11.2768272852701));
#8794=CARTESIAN_POINT('Ctrl Pts',(-3.50445479916687,11.5415837186888,10.9955772852701));
#8795=CARTESIAN_POINT('Ctrl Pts',(-3.89373205270487,10.2583010446878,10.7143272852701));
#8796=CARTESIAN_POINT('Ctrl Pts',(-5.17702162369123,9.8690180529479,10.4330772852701));
#8797=CARTESIAN_POINT('Ctrl Pts',(-6.21363996610101,10.7197633931175,10.1518272852701));
#8798=CARTESIAN_POINT('Ctrl Pts',(-6.08221720835516,12.0543226800868,9.87057728527009));
#8799=CARTESIAN_POINT('Ctrl Pts',(-4.89949422003833,12.6865022318377,9.58932728527009));
#8800=CARTESIAN_POINT('Ctrl Pts',(-3.71689478093804,12.0543000995037,9.3080772852701));
#8801=CARTESIAN_POINT('Ctrl Pts',(-3.58528891191358,10.7198194408936,9.02682728527009));
#8802=CARTESIAN_POINT('Ctrl Pts',(-4.62223822570156,9.86890150558126,8.74557728527009));
#8803=CARTESIAN_POINT('Ctrl Pts',(-5.90488911793673,10.2585344325625,8.4643272852701));
#8804=CARTESIAN_POINT('Ctrl Pts',(-6.2954241293124,11.5411191288664,8.18307728527009));
#8805=CARTESIAN_POINT('Ctrl Pts',(-5.442162067254,12.5791546772258,7.9018272852701));
#8806=CARTESIAN_POINT('Ctrl Pts',(-4.33461061966199,12.4670304559148,7.66745228527008));
#8807=CARTESIAN_POINT('Ctrl Pts',(-3.78951897521615,11.8562929714626,7.4799522852701));
#8808=CARTESIAN_POINT('Ctrl Pts',(-3.68970487524127,11.4620479800079,7.38620228527009));
#8809=CARTESIAN_POINT('Ctrl Pts',(-3.68970487524127,11.2640879581285,7.33932728527009));
#8810=CARTESIAN_POINT('Ctrl Pts',(-3.53279772223055,11.2640879581285,16.3570673917264));
#8811=CARTESIAN_POINT('Ctrl Pts',(-3.53279772223055,11.0404597227958,16.3101923917264));
#8812=CARTESIAN_POINT('Ctrl Pts',(-3.64555873781947,10.5950750170041,16.2164423917264));
#8813=CARTESIAN_POINT('Ctrl Pts',(-4.26134132595788,9.90513742653932,16.0289423917264));
#8814=CARTESIAN_POINT('Ctrl Pts',(-5.51254114817169,9.7784623284684,15.7945673917264));
#8815=CARTESIAN_POINT('Ctrl Pts',(-6.47646264640105,10.9511292017956,15.5133173917264));
#8816=CARTESIAN_POINT('Ctrl Pts',(-6.03527932038454,12.4000545169874,15.2320673917264));
#8817=CARTESIAN_POINT('Ctrl Pts',(-4.58627606607664,12.8402215235162,14.9508173917264));
#8818=CARTESIAN_POINT('Ctrl Pts',(-3.41484149286839,11.878944399442,14.6695673917264));
#8819=CARTESIAN_POINT('Ctrl Pts',(-3.56351559500105,10.371390485815,14.3883173917264));
#8820=CARTESIAN_POINT('Ctrl Pts',(-4.89949067934314,9.65719564733918,14.1070673917264));
#8821=CARTESIAN_POINT('Ctrl Pts',(-6.23560518257789,10.3713649002786,13.8258173917264));
#8822=CARTESIAN_POINT('Ctrl Pts',(-6.38407265311657,11.879007905882,13.5445673917264));
#8823=CARTESIAN_POINT('Ctrl Pts',(-5.21301156395295,12.8400894663742,13.2633173917264));
#8824=CARTESIAN_POINT('Ctrl Pts',(-3.7632875939377,12.4003189635907,12.9820673917264));
#8825=CARTESIAN_POINT('Ctrl Pts',(-3.32352358026704,10.9506027834305,12.7008173917264));
#8826=CARTESIAN_POINT('Ctrl Pts',(-4.28459682416124,9.77952884838916,12.4195673917264));
#8827=CARTESIAN_POINT('Ctrl Pts',(-5.79225398305782,9.92802041348316,12.1383173917264));
#8828=CARTESIAN_POINT('Ctrl Pts',(-6.50639642307561,11.2640879581285,11.8570673917264));
#8829=CARTESIAN_POINT('Ctrl Pts',(-5.79225398305783,12.6001555027738,11.5758173917264));
#8830=CARTESIAN_POINT('Ctrl Pts',(-4.28459682416124,12.7486470678678,11.2945673917264));
#8831=CARTESIAN_POINT('Ctrl Pts',(-3.32352358026704,11.5775731328264,11.0133173917264));
#8832=CARTESIAN_POINT('Ctrl Pts',(-3.76328759393771,10.1278569526663,10.7320673917264));
#8833=CARTESIAN_POINT('Ctrl Pts',(-5.21301156395294,9.68808644988274,10.4508173917264));
#8834=CARTESIAN_POINT('Ctrl Pts',(-6.38407265311658,10.649168010375,10.1695673917264));
#8835=CARTESIAN_POINT('Ctrl Pts',(-6.23560518257789,12.1568110159784,9.88831739172645));
#8836=CARTESIAN_POINT('Ctrl Pts',(-4.89949067934315,12.8709802689178,9.60706739172643));
#8837=CARTESIAN_POINT('Ctrl Pts',(-3.56351559500104,12.156785430442,9.32581739172646));
#8838=CARTESIAN_POINT('Ctrl Pts',(-3.41484149286839,10.649231516815,9.04456739172643));
#8839=CARTESIAN_POINT('Ctrl Pts',(-4.58627606607664,9.68795439274076,8.76331739172645));
#8840=CARTESIAN_POINT('Ctrl Pts',(-6.03527932038453,10.1281213992696,8.48206739172642));
#8841=CARTESIAN_POINT('Ctrl Pts',(-6.47646264640105,11.5770467144613,8.20081739172645));
#8842=CARTESIAN_POINT('Ctrl Pts',(-5.51254114817169,12.7497135877886,7.91956739172644));
#8843=CARTESIAN_POINT('Ctrl Pts',(-4.26134132595789,12.6230384897176,7.68519239172645));
#8844=CARTESIAN_POINT('Ctrl Pts',(-3.64555873781947,11.9331008992529,7.49769239172644));
#8845=CARTESIAN_POINT('Ctrl Pts',(-3.53279772223055,11.4877161934612,7.40394239172644));
#8846=CARTESIAN_POINT('Ctrl Pts',(-3.53279772223055,11.2640879581285,7.35706739172644));
#8847=CARTESIAN_POINT('Ctrl Pts',(-3.39185155845223,11.2640879581285,16.4968402459044));
#8848=CARTESIAN_POINT('Ctrl Pts',(-3.39185155845223,11.0174025726682,16.4499652459044));
#8849=CARTESIAN_POINT('Ctrl Pts',(-3.51624250389027,10.5260801755509,16.3562152459045));
#8850=CARTESIAN_POINT('Ctrl Pts',(-4.19552515420369,9.76499895566937,16.1687152459044));
#8851=CARTESIAN_POINT('Ctrl Pts',(-5.57576109867319,9.62525309184065,15.9343402459045));
#8852=CARTESIAN_POINT('Ctrl Pts',(-6.63908545779677,10.9188562692688,15.6530902459045));
#8853=CARTESIAN_POINT('Ctrl Pts',(-6.15240590036416,12.5172015993995,15.3718402459044));
#8854=CARTESIAN_POINT('Ctrl Pts',(-4.55397206809218,13.0027622351084,15.0905902459045));
#8855=CARTESIAN_POINT('Ctrl Pts',(-3.2617324218044,11.9423519384361,14.8093402459044));
#8856=CARTESIAN_POINT('Ctrl Pts',(-3.42573853180317,10.2793302253054,14.5280902459045));
#8857=CARTESIAN_POINT('Ctrl Pts',(-4.89948749897295,9.49148318774154,14.2468402459044));
#8858=CARTESIAN_POINT('Ctrl Pts',(-6.37339013970644,10.2793019401391,13.9655902459045));
#8859=CARTESIAN_POINT('Ctrl Pts',(-6.53716849138144,11.9424221456894,13.6843402459045));
#8860=CARTESIAN_POINT('Ctrl Pts',(-5.24534051542964,13.0026162440886,13.4030902459044));
#8861=CARTESIAN_POINT('Ctrl Pts',(-3.64611227912762,12.5174939489564,13.1218402459045));
#8862=CARTESIAN_POINT('Ctrl Pts',(-3.16099714766513,10.9182743045467,12.8405902459044));
#8863=CARTESIAN_POINT('Ctrl Pts',(-4.22118205720403,9.62643216655873,12.5593402459045));
#8864=CARTESIAN_POINT('Ctrl Pts',(-5.88431790650939,9.79023707755347,12.2780902459044));
#8865=CARTESIAN_POINT('Ctrl Pts',(-6.67210701881104,11.2640879581285,11.9968402459045));
#8866=CARTESIAN_POINT('Ctrl Pts',(-5.88431790650938,12.7379388387035,11.7155902459044));
#8867=CARTESIAN_POINT('Ctrl Pts',(-4.22118205720405,12.9017437496983,11.4343402459045));
#8868=CARTESIAN_POINT('Ctrl Pts',(-3.16099714766512,11.6099016117103,11.1530902459044));
#8869=CARTESIAN_POINT('Ctrl Pts',(-3.64611227912763,10.0106819673006,10.8718402459045));
#8870=CARTESIAN_POINT('Ctrl Pts',(-5.24534051542964,9.52555967216844,10.5905902459044));
#8871=CARTESIAN_POINT('Ctrl Pts',(-6.53716849138144,10.5857537705676,10.3093402459045));
#8872=CARTESIAN_POINT('Ctrl Pts',(-6.37339013970643,12.2488739761179,10.0280902459045));
#8873=CARTESIAN_POINT('Ctrl Pts',(-4.89948749897296,13.0366927285155,9.74684024590444));
#8874=CARTESIAN_POINT('Ctrl Pts',(-3.42573853180317,12.2488456909516,9.46559024590447));
#8875=CARTESIAN_POINT('Ctrl Pts',(-3.26173242180439,10.585823977821,9.18434024590444));
#8876=CARTESIAN_POINT('Ctrl Pts',(-4.55397206809218,9.52541368114862,8.90309024590446));
#8877=CARTESIAN_POINT('Ctrl Pts',(-6.15240590036416,10.0109743168575,8.62184024590445));
#8878=CARTESIAN_POINT('Ctrl Pts',(-6.63908545779677,11.6093196469882,8.34059024590444));
#8879=CARTESIAN_POINT('Ctrl Pts',(-5.5757610986732,12.9029228244164,8.05934024590446));
#8880=CARTESIAN_POINT('Ctrl Pts',(-4.19552515420369,12.7631769605876,7.82496524590443));
#8881=CARTESIAN_POINT('Ctrl Pts',(-3.51624250389027,12.0020957407061,7.63746524590445));
#8882=CARTESIAN_POINT('Ctrl Pts',(-3.39185155845223,11.5107733435888,7.54371524590445));
#8883=CARTESIAN_POINT('Ctrl Pts',(-3.39185155845223,11.2640879581285,7.49684024590445));
#8884=CARTESIAN_POINT('Ctrl Pts',(-3.39169253443538,11.2640879581285,16.7239318526328));
#8885=CARTESIAN_POINT('Ctrl Pts',(-3.39169253443538,11.0173582841831,16.6770568526328));
#8886=CARTESIAN_POINT('Ctrl Pts',(-3.51609209385211,10.5260079981351,16.5833068526328));
#8887=CARTESIAN_POINT('Ctrl Pts',(-4.19546021709497,9.76481862322427,16.3958068526328));
#8888=CARTESIAN_POINT('Ctrl Pts',(-5.57582838411809,9.62508432078666,16.1614318526328));
#8889=CARTESIAN_POINT('Ctrl Pts',(-6.63927771288993,10.9188140819009,15.8801818526328));
#8890=CARTESIAN_POINT('Ctrl Pts',(-6.15254061639523,12.5173402195548,15.5989318526328));
#8891=CARTESIAN_POINT('Ctrl Pts',(-4.55393526753129,13.0029501458291,15.3176818526328));
#8892=CARTESIAN_POINT('Ctrl Pts',(-3.26155390704704,11.9424263016113,15.0364318526328));
#8893=CARTESIAN_POINT('Ctrl Pts',(-3.42557844828242,10.2792228241956,14.7551818526328));
#8894=CARTESIAN_POINT('Ctrl Pts',(-4.89948739414409,9.4912905587692,14.4739318526328));
#8895=CARTESIAN_POINT('Ctrl Pts',(-6.37355048342092,10.2791947609481,14.1926818526328));
#8896=CARTESIAN_POINT('Ctrl Pts',(-6.53734656996609,11.9424959580315,13.9114318526328));
#8897=CARTESIAN_POINT('Ctrl Pts',(-5.24537813853149,13.002805300269,13.6301818526328));
#8898=CARTESIAN_POINT('Ctrl Pts',(-3.64597595622047,12.5176302748179,13.3489318526328));
#8899=CARTESIAN_POINT('Ctrl Pts',(-3.16080807547727,10.9182366901193,13.0676818526328));
#8900=CARTESIAN_POINT('Ctrl Pts',(-4.22110828163903,9.62625406348905,12.7864318526328));
#8901=CARTESIAN_POINT('Ctrl Pts',(-5.8844250104241,9.79007678593805,12.5051818526328));
#8902=CARTESIAN_POINT('Ctrl Pts',(-6.67229979784745,11.2640879581285,12.2239318526328));
#8903=CARTESIAN_POINT('Ctrl Pts',(-5.8844250104241,12.7380991303189,11.9426818526328));
#8904=CARTESIAN_POINT('Ctrl Pts',(-4.22110828163903,12.9019218527679,11.6614318526328));
#8905=CARTESIAN_POINT('Ctrl Pts',(-3.16080807547727,11.6099392261377,11.3801818526328));
#8906=CARTESIAN_POINT('Ctrl Pts',(-3.64597595622048,10.0105456414391,11.0989318526328));
#8907=CARTESIAN_POINT('Ctrl Pts',(-5.24537813853148,9.52537061598797,10.8176818526328));
#8908=CARTESIAN_POINT('Ctrl Pts',(-6.5373465699661,10.5856799582255,10.5364318526328));
#8909=CARTESIAN_POINT('Ctrl Pts',(-6.37355048342092,12.2489811553089,10.2551818526328));
#8910=CARTESIAN_POINT('Ctrl Pts',(-4.8994873941441,13.0368853574878,9.97393185263282));
#8911=CARTESIAN_POINT('Ctrl Pts',(-3.42557844828242,12.2489530920614,9.69268185263279));
#8912=CARTESIAN_POINT('Ctrl Pts',(-3.26155390704705,10.5857496146457,9.41143185263281));
#8913=CARTESIAN_POINT('Ctrl Pts',(-4.55393526753128,9.52522577042787,9.13018185263281));
#8914=CARTESIAN_POINT('Ctrl Pts',(-6.15254061639523,10.0108356967022,8.84893185263278));
#8915=CARTESIAN_POINT('Ctrl Pts',(-6.63927771288993,11.6093618343561,8.56768185263281));
#8916=CARTESIAN_POINT('Ctrl Pts',(-5.57582838411809,12.9030915954703,8.28643185263279));
#8917=CARTESIAN_POINT('Ctrl Pts',(-4.19546021709497,12.7633572930327,8.05205685263281));
#8918=CARTESIAN_POINT('Ctrl Pts',(-3.51609209385211,12.0021679181219,7.86455685263281));
#8919=CARTESIAN_POINT('Ctrl Pts',(-3.39169253443538,11.5108176320739,7.77080685263281));
#8920=CARTESIAN_POINT('Ctrl Pts',(-3.39169253443538,11.2640879581285,7.72393185263281));
#8921=CARTESIAN_POINT('Ctrl Pts',(-3.58586091972906,11.2640879581285,16.8792236164212));
#8922=CARTESIAN_POINT('Ctrl Pts',(-3.58586091972906,11.0491619105831,16.8323486164212));
#8923=CARTESIAN_POINT('Ctrl Pts',(-3.69424886155145,10.6210433711399,16.7385986164213));
#8924=CARTESIAN_POINT('Ctrl Pts',(-4.28610864698902,9.95792289030335,16.5510986164212));
#8925=CARTESIAN_POINT('Ctrl Pts',(-5.48874499113504,9.83613746089765,16.3167236164213));
#8926=CARTESIAN_POINT('Ctrl Pts',(-6.41522825428506,10.9632861137281,16.0354736164213));
#8927=CARTESIAN_POINT('Ctrl Pts',(-5.99118064031058,12.3559435166106,15.7542236164212));
#8928=CARTESIAN_POINT('Ctrl Pts',(-4.59843824494916,12.7790230813754,15.4729736164213));
#8929=CARTESIAN_POINT('Ctrl Pts',(-3.47249060193688,11.8550694784638,15.1917236164212));
#8930=CARTESIAN_POINT('Ctrl Pts',(-3.61539119000279,10.406053381894,14.9104736164213));
#8931=CARTESIAN_POINT('Ctrl Pts',(-4.89949199672205,9.71958953564843,14.6292236164212));
#8932=CARTESIAN_POINT('Ctrl Pts',(-6.18372631773713,10.4060285459761,14.3479736164213));
#8933=CARTESIAN_POINT('Ctrl Pts',(-6.3264290253672,11.8551311242623,14.0667236164213));
#8934=CARTESIAN_POINT('Ctrl Pts',(-5.20083904874642,12.7788948932607,13.7854736164212));
#8935=CARTESIAN_POINT('Ctrl Pts',(-3.80740646165742,12.3562002159562,13.5042236164213));
#8936=CARTESIAN_POINT('Ctrl Pts',(-3.38471804289437,10.9627751110632,13.2229736164213));
#8937=CARTESIAN_POINT('Ctrl Pts',(-4.30847375993061,9.83717282162548,12.9417236164213));
#8938=CARTESIAN_POINT('Ctrl Pts',(-5.75759006523555,9.97989860837387,12.6604736164212));
#8939=CARTESIAN_POINT('Ctrl Pts',(-6.44400305605043,11.2640879581285,12.3792236164213));
#8940=CARTESIAN_POINT('Ctrl Pts',(-5.75759006523555,12.5482773078831,12.0979736164212));
#8941=CARTESIAN_POINT('Ctrl Pts',(-4.30847375993062,12.6910030946315,11.8167236164213));
#8942=CARTESIAN_POINT('Ctrl Pts',(-3.38471804289437,11.5654008051937,11.5354736164212));
#8943=CARTESIAN_POINT('Ctrl Pts',(-3.80740646165742,10.1719757003009,11.2542236164213));
#8944=CARTESIAN_POINT('Ctrl Pts',(-5.20083904874642,9.74928102299629,10.9729736164213));
#8945=CARTESIAN_POINT('Ctrl Pts',(-6.3264290253672,10.6730447919947,10.6917236164212));
#8946=CARTESIAN_POINT('Ctrl Pts',(-6.18372631773713,12.1221473702809,10.4104736164213));
#8947=CARTESIAN_POINT('Ctrl Pts',(-4.89949199672205,12.8085863806086,10.1292236164212));
#8948=CARTESIAN_POINT('Ctrl Pts',(-3.61539119000279,12.122122534363,9.84797361642129));
#8949=CARTESIAN_POINT('Ctrl Pts',(-3.47249060193688,10.6731064377931,9.56672361642123));
#8950=CARTESIAN_POINT('Ctrl Pts',(-4.59843824494915,9.7491528348816,9.28547361642126));
#8951=CARTESIAN_POINT('Ctrl Pts',(-5.99118064031059,10.1722323996464,9.00422361642126));
#8952=CARTESIAN_POINT('Ctrl Pts',(-6.41522825428506,11.5648898025289,8.72297361642125));
#8953=CARTESIAN_POINT('Ctrl Pts',(-5.48874499113504,12.6920384553594,8.44172361642126));
#8954=CARTESIAN_POINT('Ctrl Pts',(-4.28610864698902,12.5702530259537,8.20734861642126));
#8955=CARTESIAN_POINT('Ctrl Pts',(-3.69424886155145,11.9071325451172,8.01984861642125));
#8956=CARTESIAN_POINT('Ctrl Pts',(-3.58586091972906,11.4790140056738,7.92609861642125));
#8957=CARTESIAN_POINT('Ctrl Pts',(-3.58586091972906,11.2640879581285,7.87922361642125));
#8958=CARTESIAN_POINT('Ctrl Pts',(-3.82797537247149,11.2640879581285,16.8235757346037));
#8959=CARTESIAN_POINT('Ctrl Pts',(-3.82797537247149,11.0887036859235,16.7767007346037));
#8960=CARTESIAN_POINT('Ctrl Pts',(-3.91636954304832,10.7395815643351,16.6829507346037));
#8961=CARTESIAN_POINT('Ctrl Pts',(-4.39919964857289,10.1985704709434,16.4954507346037));
#8962=CARTESIAN_POINT('Ctrl Pts',(-5.38013259241044,10.0993317882042,16.2610757346037));
#8963=CARTESIAN_POINT('Ctrl Pts',(-6.13590946417683,11.0187032552064,15.9798257346037));
#8964=CARTESIAN_POINT('Ctrl Pts',(-5.78999215982685,12.1547336916928,15.6985757346036));
#8965=CARTESIAN_POINT('Ctrl Pts',(-4.65392813273036,12.4998301210104,15.4173257346037));
#8966=CARTESIAN_POINT('Ctrl Pts',(-3.73547762992698,11.7461593897193,15.1360757346036));
#8967=CARTESIAN_POINT('Ctrl Pts',(-3.85204525622676,10.5641799938609,14.8548257346037));
#8968=CARTESIAN_POINT('Ctrl Pts',(-4.89949709797062,10.004226785903,14.5735757346036));
#8969=CARTESIAN_POINT('Ctrl Pts',(-5.94705958981123,10.5641605995425,14.2923257346037));
#8970=CARTESIAN_POINT('Ctrl Pts',(-6.06346322250255,11.7462075287867,14.0110757346037));
#8971=CARTESIAN_POINT('Ctrl Pts',(-5.1453091362317,12.4997300193532,13.7298257346037));
#8972=CARTESIAN_POINT('Ctrl Pts',(-4.00867310996093,12.154934145456,13.4485757346037));
#8973=CARTESIAN_POINT('Ctrl Pts',(-3.66388226535769,11.0183042408718,13.1673257346037));
#8974=CARTESIAN_POINT('Ctrl Pts',(-4.41739839453505,10.1001399894206,12.8860757346037));
#8975=CARTESIAN_POINT('Ctrl Pts',(-5.59945608391935,10.2165627311483,12.6048257346037));
#8976=CARTESIAN_POINT('Ctrl Pts',(-6.15936955148513,11.2640879581285,12.3235757346037));
#8977=CARTESIAN_POINT('Ctrl Pts',(-5.59945608391935,12.3116131851086,12.0423257346036));
#8978=CARTESIAN_POINT('Ctrl Pts',(-4.41739839453506,12.4280359268364,11.7610757346037));
#8979=CARTESIAN_POINT('Ctrl Pts',(-3.66388226535769,11.5098716753851,11.4798257346036));
#8980=CARTESIAN_POINT('Ctrl Pts',(-4.00867310996093,10.373241770801,11.1985757346037));
#8981=CARTESIAN_POINT('Ctrl Pts',(-5.14530913623169,10.0284458969038,10.9173257346037));
#8982=CARTESIAN_POINT('Ctrl Pts',(-6.06346322250255,10.7819683874703,10.6360757346037));
#8983=CARTESIAN_POINT('Ctrl Pts',(-5.94705958981124,11.9640153167145,10.3548257346037));
#8984=CARTESIAN_POINT('Ctrl Pts',(-4.89949709797062,12.523949130354,10.0735757346037));
#8985=CARTESIAN_POINT('Ctrl Pts',(-3.85204525622676,11.9639959223961,9.79232573460369));
#8986=CARTESIAN_POINT('Ctrl Pts',(-3.73547762992698,10.7820165265377,9.51107573460366));
#8987=CARTESIAN_POINT('Ctrl Pts',(-4.65392813273036,10.0283457952466,9.22982573460369));
#8988=CARTESIAN_POINT('Ctrl Pts',(-5.78999215982684,10.3734422245642,8.94857573460365));
#8989=CARTESIAN_POINT('Ctrl Pts',(-6.13590946417682,11.5094726610506,8.66732573460368));
#8990=CARTESIAN_POINT('Ctrl Pts',(-5.38013259241045,12.4288441280527,8.38607573460367));
#8991=CARTESIAN_POINT('Ctrl Pts',(-4.39919964857288,12.3296054453136,8.15170073460366));
#8992=CARTESIAN_POINT('Ctrl Pts',(-3.91636954304832,11.7885943519219,7.96420073460368));
#8993=CARTESIAN_POINT('Ctrl Pts',(-3.82797537247149,11.4394722303336,7.87045073460367));
#8994=CARTESIAN_POINT('Ctrl Pts',(-3.82797537247149,11.2640879581285,7.82357573460367));
#8995=CARTESIAN_POINT('Ctrl Pts',(-3.89952178519528,11.2640879581285,16.6747998250855));
#8996=CARTESIAN_POINT('Ctrl Pts',(-3.89952178519528,11.1005833965992,16.6279248250855));
#8997=CARTESIAN_POINT('Ctrl Pts',(-3.98205572967308,10.7745499551565,16.5341748250855));
#8998=CARTESIAN_POINT('Ctrl Pts',(-4.43251939644262,10.2699203425333,16.3466748250855));
#8999=CARTESIAN_POINT('Ctrl Pts',(-5.34808002652064,10.1770638423901,16.1122998250855));
#9000=CARTESIAN_POINT('Ctrl Pts',(-6.05327536604636,11.0351409647361,15.8310498250855));
#9001=CARTESIAN_POINT('Ctrl Pts',(-5.73051227207975,12.0952061134392,15.5497998250855));
#9002=CARTESIAN_POINT('Ctrl Pts',(-4.67032952591772,12.4172785427992,15.2685498250855));
#9003=CARTESIAN_POINT('Ctrl Pts',(-3.81325352813639,11.7139456413251,14.9872998250855));
#9004=CARTESIAN_POINT('Ctrl Pts',(-3.92202751272141,10.610945121295,14.7060498250855));
#9005=CARTESIAN_POINT('Ctrl Pts',(-4.89949968495297,10.0883993401394,14.4247998250855));
#9006=CARTESIAN_POINT('Ctrl Pts',(-5.87707091221916,10.6109249362026,14.1435498250855));
#9007=CARTESIAN_POINT('Ctrl Pts',(-5.98569808817465,11.7139957432225,13.8622998250855));
#9008=CARTESIAN_POINT('Ctrl Pts',(-5.12888744491114,12.4171743591843,13.5810498250855));
#9009=CARTESIAN_POINT('Ctrl Pts',(-4.06819264464732,12.0954147460485,13.2997998250855));
#9010=CARTESIAN_POINT('Ctrl Pts',(-3.74643790785961,11.0347256140874,13.0185498250855));
#9011=CARTESIAN_POINT('Ctrl Pts',(-4.44961008867104,10.1779057780296,12.7372998250855));
#9012=CARTESIAN_POINT('Ctrl Pts',(-5.55269199185788,10.2865501028716,12.4560498250855));
#9013=CARTESIAN_POINT('Ctrl Pts',(-6.07519648156484,11.2640879581285,12.1747998250855));
#9014=CARTESIAN_POINT('Ctrl Pts',(-5.55269199185788,12.2416258133854,11.8935498250855));
#9015=CARTESIAN_POINT('Ctrl Pts',(-4.44961008867105,12.3502701382274,11.6122998250855));
#9016=CARTESIAN_POINT('Ctrl Pts',(-3.74643790785961,11.4934503021696,11.3310498250855));
#9017=CARTESIAN_POINT('Ctrl Pts',(-4.06819264464732,10.4327611702086,11.0497998250855));
#9018=CARTESIAN_POINT('Ctrl Pts',(-5.12888744491114,10.1110015570726,10.7685498250855));
#9019=CARTESIAN_POINT('Ctrl Pts',(-5.98569808817465,10.8141801730346,10.4872998250855));
#9020=CARTESIAN_POINT('Ctrl Pts',(-5.87707091221916,11.9172509800544,10.2060498250855));
#9021=CARTESIAN_POINT('Ctrl Pts',(-4.89949968495297,12.4397765761176,9.92479982508546));
#9022=CARTESIAN_POINT('Ctrl Pts',(-3.92202751272141,11.9172307949619,9.64354982508548));
#9023=CARTESIAN_POINT('Ctrl Pts',(-3.81325352813639,10.8142302749319,9.36229982508546));
#9024=CARTESIAN_POINT('Ctrl Pts',(-4.67032952591772,10.1108973734578,9.08104982508548));
#9025=CARTESIAN_POINT('Ctrl Pts',(-5.73051227207974,10.4329698028178,8.79979982508546));
#9026=CARTESIAN_POINT('Ctrl Pts',(-6.05327536604636,11.4930349515209,8.51854982508547));
#9027=CARTESIAN_POINT('Ctrl Pts',(-5.34808002652064,12.3511120738669,8.23729982508547));
#9028=CARTESIAN_POINT('Ctrl Pts',(-4.43251939644262,12.2582555737237,8.00292482508547));
#9029=CARTESIAN_POINT('Ctrl Pts',(-3.98205572967307,11.7536259611005,7.81542482508547));
#9030=CARTESIAN_POINT('Ctrl Pts',(-3.89952178519528,11.4275925196578,7.72167482508547));
#9031=CARTESIAN_POINT('Ctrl Pts',(-3.89952178519528,11.2640879581285,7.67479982508547));
#9032=CARTESIAN_POINT('Ctrl Pts',(-3.89952178519528,11.2640879581285,16.6));
#9033=CARTESIAN_POINT('Ctrl Pts',(-3.89952178519528,11.100463340754,16.553125));
#9034=CARTESIAN_POINT('Ctrl Pts',(-3.98202611573229,10.7745871843551,16.459375));
#9035=CARTESIAN_POINT('Ctrl Pts',(-4.43258063114212,10.2697743643378,16.271875));
#9036=CARTESIAN_POINT('Ctrl Pts',(-5.34805346405984,10.1770907055197,16.0375));
#9037=CARTESIAN_POINT('Ctrl Pts',(-6.05333301021299,11.0351030238058,15.75625));
#9038=CARTESIAN_POINT('Ctrl Pts',(-5.7305291347766,12.0952484733215,15.475));
#9039=CARTESIAN_POINT('Ctrl Pts',(-4.67032720528385,12.41730825404,15.19375));
#9040=CARTESIAN_POINT('Ctrl Pts',(-3.81321563500956,11.71396418737,14.9125));
#9041=CARTESIAN_POINT('Ctrl Pts',(-3.92199706138937,10.6109219094395,14.63125));
#9042=CARTESIAN_POINT('Ctrl Pts',(-4.89949901982681,10.0883621413897,14.35));
#9043=CARTESIAN_POINT('Ctrl Pts',(-5.87710301444863,10.6109032023111,14.06875));
#9044=CARTESIAN_POINT('Ctrl Pts',(-5.98573321383868,11.7140106207574,13.7875));
#9045=CARTESIAN_POINT('Ctrl Pts',(-5.12889498447605,12.4172116991036,13.50625));
#9046=CARTESIAN_POINT('Ctrl Pts',(-4.06816558640322,12.095441826144,13.225));
#9047=CARTESIAN_POINT('Ctrl Pts',(-3.74640046021744,11.0347181280085,12.94375));
#9048=CARTESIAN_POINT('Ctrl Pts',(-4.44959545666081,10.177870497758,12.6625));
#9049=CARTESIAN_POINT('Ctrl Pts',(-5.55271322406204,10.2865183309037,12.38125));
#9050=CARTESIAN_POINT('Ctrl Pts',(-6.07523468001534,11.2640879581285,12.1));
#9051=CARTESIAN_POINT('Ctrl Pts',(-5.55271322406204,12.2416575853533,11.81875));
#9052=CARTESIAN_POINT('Ctrl Pts',(-4.44959545666081,12.3503054184991,11.5375));
#9053=CARTESIAN_POINT('Ctrl Pts',(-3.74640046021743,11.4934577882485,11.25625));
#9054=CARTESIAN_POINT('Ctrl Pts',(-4.06816558640323,10.432734090113,10.975));
#9055=CARTESIAN_POINT('Ctrl Pts',(-5.12889498447604,10.1109642171534,10.69375));
#9056=CARTESIAN_POINT('Ctrl Pts',(-5.98573321383869,10.8141652954996,10.4125));
#9057=CARTESIAN_POINT('Ctrl Pts',(-5.87710301444862,11.9172727139459,10.13125));
#9058=CARTESIAN_POINT('Ctrl Pts',(-4.89949901982682,12.4398137748673,9.85));
#9059=CARTESIAN_POINT('Ctrl Pts',(-3.92199706138938,11.9172540068175,9.56875));
#9060=CARTESIAN_POINT('Ctrl Pts',(-3.81321563500956,10.8142117288869,9.2875));
#9061=CARTESIAN_POINT('Ctrl Pts',(-4.67032720528385,10.110867662217,9.00625));
#9062=CARTESIAN_POINT('Ctrl Pts',(-5.73052913477659,10.4329274429355,8.725));
#9063=CARTESIAN_POINT('Ctrl Pts',(-6.05333301021299,11.4930728924512,8.44374999999999));
#9064=CARTESIAN_POINT('Ctrl Pts',(-5.34805346405984,12.3510852107373,8.16250000000001));
#9065=CARTESIAN_POINT('Ctrl Pts',(-4.43258063114213,12.2584015519192,7.92812499999999));
#9066=CARTESIAN_POINT('Ctrl Pts',(-3.98202611573229,11.7535887319019,7.740625));
#9067=CARTESIAN_POINT('Ctrl Pts',(-3.89952178519528,11.427712575503,7.646875));
#9068=CARTESIAN_POINT('Ctrl Pts',(-3.89952178519528,11.2640879581285,7.6));
#9069=CARTESIAN_POINT('',(-3.89952178519528,11.2640879581285,7.6));
#9070=CARTESIAN_POINT('Ctrl Pts',(-3.89952178519528,11.2640879581285,16.6));
#9071=CARTESIAN_POINT('Ctrl Pts',(-3.89952178519528,11.100463340754,16.553125));
#9072=CARTESIAN_POINT('Ctrl Pts',(-3.98202611573229,10.7745871843551,16.459375));
#9073=CARTESIAN_POINT('Ctrl Pts',(-4.43258063114212,10.2697743643378,16.271875));
#9074=CARTESIAN_POINT('Ctrl Pts',(-5.34805346405984,10.1770907055197,16.0375));
#9075=CARTESIAN_POINT('Ctrl Pts',(-6.05333301021299,11.0351030238058,15.75625));
#9076=CARTESIAN_POINT('Ctrl Pts',(-5.7305291347766,12.0952484733215,15.475));
#9077=CARTESIAN_POINT('Ctrl Pts',(-4.67032720528385,12.41730825404,15.19375));
#9078=CARTESIAN_POINT('Ctrl Pts',(-3.81321563500956,11.71396418737,14.9125));
#9079=CARTESIAN_POINT('Ctrl Pts',(-3.92199706138937,10.6109219094395,14.63125));
#9080=CARTESIAN_POINT('Ctrl Pts',(-4.89949901982681,10.0883621413897,14.35));
#9081=CARTESIAN_POINT('Ctrl Pts',(-5.87710301444863,10.6109032023111,14.06875));
#9082=CARTESIAN_POINT('Ctrl Pts',(-5.98573321383868,11.7140106207574,13.7875));
#9083=CARTESIAN_POINT('Ctrl Pts',(-5.12889498447605,12.4172116991036,13.50625));
#9084=CARTESIAN_POINT('Ctrl Pts',(-4.06816558640322,12.095441826144,13.225));
#9085=CARTESIAN_POINT('Ctrl Pts',(-3.74640046021744,11.0347181280085,12.94375));
#9086=CARTESIAN_POINT('Ctrl Pts',(-4.44959545666081,10.177870497758,12.6625));
#9087=CARTESIAN_POINT('Ctrl Pts',(-5.55271322406204,10.2865183309037,12.38125));
#9088=CARTESIAN_POINT('Ctrl Pts',(-6.07523468001534,11.2640879581285,12.1));
#9089=CARTESIAN_POINT('Ctrl Pts',(-5.55271322406204,12.2416575853533,11.81875));
#9090=CARTESIAN_POINT('Ctrl Pts',(-4.44959545666081,12.3503054184991,11.5375));
#9091=CARTESIAN_POINT('Ctrl Pts',(-3.74640046021743,11.4934577882485,11.25625));
#9092=CARTESIAN_POINT('Ctrl Pts',(-4.06816558640323,10.432734090113,10.975));
#9093=CARTESIAN_POINT('Ctrl Pts',(-5.12889498447604,10.1109642171534,10.69375));
#9094=CARTESIAN_POINT('Ctrl Pts',(-5.98573321383869,10.8141652954996,10.4125));
#9095=CARTESIAN_POINT('Ctrl Pts',(-5.87710301444862,11.9172727139459,10.13125));
#9096=CARTESIAN_POINT('Ctrl Pts',(-4.89949901982682,12.4398137748673,9.85));
#9097=CARTESIAN_POINT('Ctrl Pts',(-3.92199706138938,11.9172540068175,9.56875));
#9098=CARTESIAN_POINT('Ctrl Pts',(-3.81321563500956,10.8142117288869,9.2875));
#9099=CARTESIAN_POINT('Ctrl Pts',(-4.67032720528385,10.110867662217,9.00625));
#9100=CARTESIAN_POINT('Ctrl Pts',(-5.73052913477659,10.4329274429355,8.725));
#9101=CARTESIAN_POINT('Ctrl Pts',(-6.05333301021299,11.4930728924512,8.44374999999999));
#9102=CARTESIAN_POINT('Ctrl Pts',(-5.34805346405984,12.3510852107373,8.16250000000001));
#9103=CARTESIAN_POINT('Ctrl Pts',(-4.43258063114213,12.2584015519192,7.92812499999999));
#9104=CARTESIAN_POINT('Ctrl Pts',(-3.98202611573229,11.7535887319019,7.740625));
#9105=CARTESIAN_POINT('Ctrl Pts',(-3.89952178519528,11.427712575503,7.646875));
#9106=CARTESIAN_POINT('Ctrl Pts',(-3.89952178519528,11.2640879581285,7.6));
#9107=CARTESIAN_POINT('Origin',(-3.64952178519528,11.2640879581285,7.6));
#9108=CARTESIAN_POINT('Origin',(-3.64952178519528,11.2640879581285,7.6));
#9109=CARTESIAN_POINT('',(0.,0.,0.));
#9110=CARTESIAN_POINT('Origin',(-4.88927830720691,25.1107216927931,9.2));
#9111=CARTESIAN_POINT('',(-7.48735451856023,25.1107216927931,7.7));
#9112=CARTESIAN_POINT('Origin',(-4.88927830720691,25.1107216927931,7.7));
#9113=CARTESIAN_POINT('',(-4.88927830720691,25.1107216927931,6.2));
#9114=CARTESIAN_POINT('Origin',(-4.88927830720691,25.1107216927931,9.2));
#9115=CARTESIAN_POINT('Origin',(-4.88927830720691,25.1107216927931,8.2));
#9116=CARTESIAN_POINT('',(-7.54689383586007,25.1107216927931,7.7));
#9117=CARTESIAN_POINT('Origin',(-4.88927830720691,25.1107216927931,7.7));
#9118=CARTESIAN_POINT('',(-8.04689383586007,25.1107216927931,8.2));
#9119=CARTESIAN_POINT('Origin',(-7.54689383586007,25.1107216927931,8.2));
#9120=CARTESIAN_POINT('Origin',(-4.88927830720691,25.1107216927931,8.2));
#9121=CARTESIAN_POINT('Origin',(-4.88927830720691,25.1107216927931,19.));
#9122=CARTESIAN_POINT('',(-8.04689383586007,25.1107216927931,18.5));
#9123=CARTESIAN_POINT('',(-8.04689383586007,25.1107216927931,19.));
#9124=CARTESIAN_POINT('Origin',(-4.88927830720691,25.1107216927931,18.5));
#9125=CARTESIAN_POINT('Origin',(-4.88927830720691,25.1107216927931,7.7));
#9126=CARTESIAN_POINT('Origin',(-4.88927830720691,23.3786708852242,19.));
#9127=CARTESIAN_POINT('',(-4.88927830720691,23.3786708852242,19.));
#9128=CARTESIAN_POINT('',(-6.38927830720691,24.2446962890086,19.));
#9129=CARTESIAN_POINT('',(-5.26427830720691,23.5951772361703,19.));
#9130=CARTESIAN_POINT('',(-4.88927830720691,23.3786708852242,18.));
#9131=CARTESIAN_POINT('',(-4.88927830720691,23.3786708852242,19.));
#9132=CARTESIAN_POINT('',(-6.38927830720691,24.2446962890086,18.));
#9133=CARTESIAN_POINT('',(-6.38927830720691,24.2446962890086,18.));
#9134=CARTESIAN_POINT('',(-6.38927830720691,24.2446962890086,19.));
#9135=CARTESIAN_POINT('Origin',(-3.38927830720691,24.2446962890086,19.));
#9136=CARTESIAN_POINT('',(-3.38927830720691,24.2446962890086,19.));
#9137=CARTESIAN_POINT('',(-3.76427830720691,24.0281899380625,19.));
#9138=CARTESIAN_POINT('',(-3.38927830720691,24.2446962890086,18.));
#9139=CARTESIAN_POINT('',(-3.38927830720691,24.2446962890086,19.));
#9140=CARTESIAN_POINT('',(-4.88927830720691,23.3786708852242,18.));
#9141=CARTESIAN_POINT('Origin',(-3.38927830720691,25.9767470965775,19.));
#9142=CARTESIAN_POINT('',(-3.38927830720691,25.9767470965775,19.));
#9143=CARTESIAN_POINT('',(-3.38927830720691,25.5437343946853,19.));
#9144=CARTESIAN_POINT('',(-3.38927830720691,25.9767470965775,18.));
#9145=CARTESIAN_POINT('',(-3.38927830720691,25.9767470965775,19.));
#9146=CARTESIAN_POINT('',(-3.38927830720691,24.2446962890086,18.));
#9147=CARTESIAN_POINT('Origin',(-4.88927830720691,26.842772500362,19.));
#9148=CARTESIAN_POINT('',(-4.88927830720691,26.842772500362,19.));
#9149=CARTESIAN_POINT('',(-4.51427830720691,26.6262661494159,19.));
#9150=CARTESIAN_POINT('',(-4.88927830720691,26.842772500362,18.));
#9151=CARTESIAN_POINT('',(-4.88927830720691,26.842772500362,19.));
#9152=CARTESIAN_POINT('',(-3.38927830720691,25.9767470965775,18.));
#9153=CARTESIAN_POINT('Origin',(-6.38927830720691,25.9767470965775,19.));
#9154=CARTESIAN_POINT('',(-6.38927830720691,25.9767470965775,19.));
#9155=CARTESIAN_POINT('',(-6.01427830720691,26.1932534475236,19.));
#9156=CARTESIAN_POINT('',(-6.38927830720691,25.9767470965775,18.));
#9157=CARTESIAN_POINT('',(-6.38927830720691,25.9767470965775,19.));
#9158=CARTESIAN_POINT('',(-4.88927830720691,26.842772500362,18.));
#9159=CARTESIAN_POINT('Origin',(-6.38927830720691,24.2446962890086,19.));
#9160=CARTESIAN_POINT('',(-6.38927830720691,24.6777089909009,19.));
#9161=CARTESIAN_POINT('',(-6.38927830720691,25.9767470965775,18.));
#9162=CARTESIAN_POINT('Origin',(-4.88927830720691,25.1107216927931,18.));
#9163=CARTESIAN_POINT('Origin',(-4.88927830720691,25.1107216927931,18.75));
#9164=CARTESIAN_POINT('',(-7.54689383586007,25.1107216927931,19.));
#9165=CARTESIAN_POINT('Origin',(-4.88927830720691,25.1107216927931,19.));
#9166=CARTESIAN_POINT('',(-7.79689383586007,25.1107216927931,18.75));
#9167=CARTESIAN_POINT('Origin',(-4.88927830720691,25.1107216927931,19.));
#9168=CARTESIAN_POINT('',(0.,0.,0.));
#9169=CARTESIAN_POINT('Origin',(-4.88927830720691,5.31072169279307,9.2));
#9170=CARTESIAN_POINT('',(-7.48735451856022,5.31072169279307,7.7));
#9171=CARTESIAN_POINT('Origin',(-4.88927830720691,5.31072169279307,7.7));
#9172=CARTESIAN_POINT('',(-4.88927830720691,5.31072169279307,6.2));
#9173=CARTESIAN_POINT('Origin',(-4.88927830720691,5.31072169279307,9.2));
#9174=CARTESIAN_POINT('Origin',(-11.4815115348679,14.3472131187871,7.7));
#9175=CARTESIAN_POINT('',(-1.50492583139032,3.29514581742751,7.7));
#9176=CARTESIAN_POINT('',(-3.54346119653592,1.3536835649079,7.69999999999999));
#9177=CARTESIAN_POINT('',(-1.20576175806249,3.58006398250164,7.7));
#9178=CARTESIAN_POINT('',(-1.34975341759722,3.65721478294476,7.7));
#9179=CARTESIAN_POINT('Origin',(-1.84975341759722,3.65721478294476,7.7));
#9180=CARTESIAN_POINT('',(-1.34975341759722,25.1502465824028,7.7));
#9181=CARTESIAN_POINT('',(-1.34975341759722,19.7487298505949,7.7));
#9182=CARTESIAN_POINT('',(-4.84975341759722,28.6502465824028,7.7));
#9183=CARTESIAN_POINT('Origin',(-4.84975341759722,25.1502465824028,7.7));
#9184=CARTESIAN_POINT('',(-26.3427852170552,28.6502465824028,7.7));
#9185=CARTESIAN_POINT('',(-8.16563247623254,28.6502465824028,7.7));
#9186=CARTESIAN_POINT('',(-26.7048541825725,28.4950741686097,7.7));
#9187=CARTESIAN_POINT('Origin',(-26.3427852170552,28.1502465824028,7.7));
#9188=CARTESIAN_POINT('',(-28.6463164350921,26.4565388034641,7.7));
#9189=CARTESIAN_POINT('',(-26.4695350109151,28.74215929885,7.7));
#9190=CARTESIAN_POINT('',(-28.7842474695749,26.1117112172572,7.7));
#9191=CARTESIAN_POINT('Origin',(-28.2842474695748,26.1117112172572,7.7));
#9192=CARTESIAN_POINT('',(-28.7842474695749,24.1035614526515,7.7));
#9193=CARTESIAN_POINT('',(-28.7842474695749,20.4294621680221,7.7));
#9194=CARTESIAN_POINT('',(-28.6378008601681,23.7500080620583,7.7));
#9195=CARTESIAN_POINT('Origin',(-28.2842474695748,24.1035614526515,7.7));
#9196=CARTESIAN_POINT('',(-26.5545620724644,21.6667692743546,7.7));
#9197=CARTESIAN_POINT('',(-22.144476402432,17.2566836043221,7.7));
#9198=CARTESIAN_POINT('',(-26.2010086818712,21.5203226649479,7.7));
#9199=CARTESIAN_POINT('Origin',(-26.2010086818712,22.0203226649479,7.7));
#9200=CARTESIAN_POINT('',(-24.6787384375659,21.5203226649479,7.7));
#9201=CARTESIAN_POINT('',(-19.0483668895561,21.5203226649479,7.7));
#9202=CARTESIAN_POINT('',(-23.2398888132926,16.9758883278442,7.7));
#9203=CARTESIAN_POINT('Origin',(-24.6787384375659,19.0203226649479,7.7));
#9204=CARTESIAN_POINT('',(-23.452118888438,16.5670014604234,7.7));
#9205=CARTESIAN_POINT('Origin',(-22.952118888438,16.5670014604234,7.7));
#9206=CARTESIAN_POINT('',(-23.452118888438,10.1397931465341,7.7));
#9207=CARTESIAN_POINT('',(-23.452118888438,15.7520994917882,7.7));
#9208=CARTESIAN_POINT('',(-23.3056722790312,9.78623975594079,7.7));
#9209=CARTESIAN_POINT('Origin',(-22.952118888438,10.1397931465341,7.7));
#9210=CARTESIAN_POINT('',(-20.2137602440592,6.69432772096875,7.7));
#9211=CARTESIAN_POINT('',(-19.7974728068092,6.27804028371878,7.7));
#9212=CARTESIAN_POINT('',(-19.8602068534659,6.54788111156203,7.7));
#9213=CARTESIAN_POINT('Origin',(-19.8602068534659,7.04788111156203,7.7));
#9214=CARTESIAN_POINT('',(-13.4329985395765,6.54788111156204,7.7));
#9215=CARTESIAN_POINT('',(-12.1622628350393,6.54788111156203,7.7));
#9216=CARTESIAN_POINT('',(-13.0241116721558,6.76011118670738,7.7));
#9217=CARTESIAN_POINT('Origin',(-13.4329985395765,7.04788111156204,7.7));
#9218=CARTESIAN_POINT('',(-8.47967733505213,5.32126156243407,7.7));
#9219=CARTESIAN_POINT('Origin',(-10.9796773350521,5.32126156243407,7.7));
#9220=CARTESIAN_POINT('',(-8.47967733505213,3.79899131812881,7.7));
#9221=CARTESIAN_POINT('',(-8.47967733505213,8.86599543727138,7.7));
#9222=CARTESIAN_POINT('',(-8.3332307256454,3.44543792753554,7.7));
#9223=CARTESIAN_POINT('Origin',(-7.97967733505213,3.79899131812881,7.7));
#9224=CARTESIAN_POINT('',(-6.24999193794173,1.36219913983186,7.69999999999999));
#9225=CARTESIAN_POINT('',(-10.6576787225053,5.76988592439547,7.7));
#9226=CARTESIAN_POINT('',(-5.89643854734845,1.21575253042514,7.69999999999999));
#9227=CARTESIAN_POINT('Origin',(-5.89643854734845,1.71575253042514,7.69999999999999));
#9228=CARTESIAN_POINT('',(-3.88828878274281,1.21575253042514,7.69999999999999));
#9229=CARTESIAN_POINT('',(-7.48490015880533,1.21575253042514,7.69999999999999));
#9230=CARTESIAN_POINT('Origin',(-3.88828878274281,1.71575253042514,7.69999999999999));
#9231=CARTESIAN_POINT('',(-10.8648573190427,23.3513464861378,7.7));
#9232=CARTESIAN_POINT('Origin',(-10.8648573190427,25.1013464861378,7.7));
#9233=CARTESIAN_POINT('',(-6.64865351386214,11.2651426809573,7.7));
#9234=CARTESIAN_POINT('Origin',(-4.89865351386214,11.2651426809573,7.7));
#9235=CARTESIAN_POINT('',(-20.801482994706,15.198517005294,7.7));
#9236=CARTESIAN_POINT('Origin',(-14.801482994706,15.198517005294,7.7));
#9237=CARTESIAN_POINT('',(-6.64865351386214,19.1351426809573,7.7));
#9238=CARTESIAN_POINT('Origin',(-4.89865351386214,19.1351426809573,7.7));
#9239=CARTESIAN_POINT('',(-18.7348573190427,23.3513464861378,7.7));
#9240=CARTESIAN_POINT('Origin',(-18.7348573190427,25.1013464861378,7.7));
#9241=CARTESIAN_POINT('',(-27.2873545185602,25.1107216927931,7.7));
#9242=CARTESIAN_POINT('Origin',(-24.6892783072069,25.1107216927931,7.7));
#9243=CARTESIAN_POINT('',(-7.48735451856023,25.1107216927931,7.7));
#9244=CARTESIAN_POINT('Origin',(-4.88927830720691,25.1107216927931,7.7));
#9245=CARTESIAN_POINT('Origin',(-4.88927830720691,25.1107216927931,9.2));
#9246=CARTESIAN_POINT('',(-4.88927830720691,25.1107216927931,6.2));
#9247=CARTESIAN_POINT('Origin',(-4.88927830720691,25.1107216927931,9.2));
#9248=CARTESIAN_POINT('Origin',(-24.6892783072069,25.1107216927931,9.2));
#9249=CARTESIAN_POINT('',(-24.6892783072069,25.1107216927931,6.2));
#9250=CARTESIAN_POINT('Origin',(-24.6892783072069,25.1107216927931,9.2));
#9251=CARTESIAN_POINT('Origin',(-18.7348573190427,25.1013464861378,7.45));
#9252=CARTESIAN_POINT('',(-18.7348573190427,23.8513464861378,7.2));
#9253=CARTESIAN_POINT('',(-18.7348573190427,23.6013464861378,7.45));
#9254=CARTESIAN_POINT('Origin',(-18.7348573190427,25.1013464861378,7.2));
#9255=CARTESIAN_POINT('Origin',(-18.7348573190427,25.1013464861378,19.));
#9256=CARTESIAN_POINT('',(-18.7348573190427,23.8513464861378,1.1));
#9257=CARTESIAN_POINT('Origin',(-18.7348573190427,25.1013464861378,1.1));
#9258=CARTESIAN_POINT('',(-18.7348573190427,23.8513464861378,19.));
#9259=CARTESIAN_POINT('Origin',(-10.8648573190427,25.1013464861379,7.45));
#9260=CARTESIAN_POINT('',(-10.8648573190427,23.8513464861378,7.2));
#9261=CARTESIAN_POINT('',(-10.8648573190427,23.6013464861379,7.45));
#9262=CARTESIAN_POINT('Origin',(-10.8648573190427,25.1013464861379,7.2));
#9263=CARTESIAN_POINT('Origin',(-10.8648573190427,25.1013464861378,19.));
#9264=CARTESIAN_POINT('',(-10.8648573190427,23.8513464861379,1.1));
#9265=CARTESIAN_POINT('Origin',(-10.8648573190427,25.1013464861379,1.1));
#9266=CARTESIAN_POINT('',(-10.8648573190427,23.8513464861378,19.));
#9267=CARTESIAN_POINT('Origin',(-4.89865351386214,19.1351426809573,7.45));
#9268=CARTESIAN_POINT('',(-6.14865351386214,19.1351426809573,7.2));
#9269=CARTESIAN_POINT('Origin',(-4.89865351386214,19.1351426809573,7.2));
#9270=CARTESIAN_POINT('',(-6.39865351386215,19.1351426809573,7.45));
#9271=CARTESIAN_POINT('Origin',(-4.89865351386214,19.1351426809573,19.));
#9272=CARTESIAN_POINT('',(-6.14865351386214,19.1351426809573,1.1));
#9273=CARTESIAN_POINT('Origin',(-4.89865351386214,19.1351426809573,1.1));
#9274=CARTESIAN_POINT('',(-6.14865351386214,19.1351426809573,19.));
#9275=CARTESIAN_POINT('Origin',(-4.89865351386214,11.2651426809573,7.45));
#9276=CARTESIAN_POINT('',(-6.14865351386214,11.2651426809573,7.2));
#9277=CARTESIAN_POINT('Origin',(-4.89865351386214,11.2651426809573,7.2));
#9278=CARTESIAN_POINT('',(-6.39865351386215,11.2651426809573,7.45));
#9279=CARTESIAN_POINT('Origin',(-4.89865351386214,11.2651426809573,19.));
#9280=CARTESIAN_POINT('',(-6.14865351386214,11.2651426809573,1.1));
#9281=CARTESIAN_POINT('Origin',(-4.89865351386214,11.2651426809573,1.1));
#9282=CARTESIAN_POINT('',(-6.14865351386214,11.2651426809573,19.));
#9283=CARTESIAN_POINT('Origin',(-18.7348573190427,25.1013464861378,0.850000000000002));
#9284=CARTESIAN_POINT('',(-18.7348573190427,23.3513464861378,0.600000000000003));
#9285=CARTESIAN_POINT('',(-18.7348573190427,23.6013464861378,0.850000000000002));
#9286=CARTESIAN_POINT('Origin',(-18.7348573190427,25.1013464861378,0.600000000000003));
#9287=CARTESIAN_POINT('Origin',(-11.4815115348679,14.3472131187871,0.600000000000001));
#9288=CARTESIAN_POINT('',(-3.54346119653592,1.35368356490791,0.599999999999998));
#9289=CARTESIAN_POINT('',(-1.50492583139032,3.29514581742752,0.600000000000001));
#9290=CARTESIAN_POINT('',(-1.20576175806249,3.58006398250165,0.600000000000001));
#9291=CARTESIAN_POINT('',(-3.88828878274281,1.21575253042515,0.599999999999998));
#9292=CARTESIAN_POINT('Origin',(-3.88828878274281,1.71575253042515,0.599999999999998));
#9293=CARTESIAN_POINT('',(-5.89643854734845,1.21575253042515,0.599999999999998));
#9294=CARTESIAN_POINT('',(-7.48490015880533,1.21575253042515,0.599999999999998));
#9295=CARTESIAN_POINT('',(-6.24999193794173,1.36219913983187,0.599999999999998));
#9296=CARTESIAN_POINT('Origin',(-5.89643854734845,1.71575253042515,0.599999999999998));
#9297=CARTESIAN_POINT('',(-8.3332307256454,3.44543792753555,0.600000000000001));
#9298=CARTESIAN_POINT('',(-10.6576787225053,5.76988592439548,0.600000000000001));
#9299=CARTESIAN_POINT('',(-8.47967733505213,3.79899131812882,0.600000000000001));
#9300=CARTESIAN_POINT('Origin',(-7.97967733505213,3.79899131812882,0.600000000000001));
#9301=CARTESIAN_POINT('',(-8.47967733505213,5.32126156243408,0.600000000000001));
#9302=CARTESIAN_POINT('',(-8.47967733505213,8.86599543727139,0.600000000000001));
#9303=CARTESIAN_POINT('',(-13.0241116721558,6.76011118670738,0.600000000000001));
#9304=CARTESIAN_POINT('Origin',(-10.9796773350521,5.32126156243408,0.600000000000001));
#9305=CARTESIAN_POINT('',(-13.4329985395765,6.54788111156205,0.600000000000001));
#9306=CARTESIAN_POINT('Origin',(-13.4329985395765,7.04788111156204,0.600000000000001));
#9307=CARTESIAN_POINT('',(-19.8602068534659,6.54788111156204,0.600000000000001));
#9308=CARTESIAN_POINT('',(-12.1622628350393,6.54788111156204,0.600000000000001));
#9309=CARTESIAN_POINT('',(-20.2137602440592,6.69432772096876,0.600000000000001));
#9310=CARTESIAN_POINT('Origin',(-19.8602068534659,7.04788111156204,0.600000000000001));
#9311=CARTESIAN_POINT('',(-23.3056722790312,9.7862397559408,0.600000000000001));
#9312=CARTESIAN_POINT('',(-19.7974728068092,6.27804028371878,0.600000000000001));
#9313=CARTESIAN_POINT('',(-23.452118888438,10.1397931465341,0.600000000000001));
#9314=CARTESIAN_POINT('Origin',(-22.952118888438,10.1397931465341,0.600000000000001));
#9315=CARTESIAN_POINT('',(-23.452118888438,16.5670014604234,0.600000000000001));
#9316=CARTESIAN_POINT('',(-23.452118888438,15.7520994917882,0.600000000000001));
#9317=CARTESIAN_POINT('',(-23.2398888132926,16.9758883278442,0.600000000000001));
#9318=CARTESIAN_POINT('Origin',(-22.952118888438,16.5670014604234,0.600000000000001));
#9319=CARTESIAN_POINT('',(-24.6787384375659,21.5203226649479,0.600000000000003));
#9320=CARTESIAN_POINT('Origin',(-24.6787384375659,19.0203226649479,0.600000000000001));
#9321=CARTESIAN_POINT('',(-26.2010086818712,21.5203226649479,0.600000000000003));
#9322=CARTESIAN_POINT('',(-19.0483668895561,21.5203226649479,0.600000000000003));
#9323=CARTESIAN_POINT('',(-26.5545620724644,21.6667692743546,0.600000000000003));
#9324=CARTESIAN_POINT('Origin',(-26.2010086818712,22.0203226649479,0.600000000000003));
#9325=CARTESIAN_POINT('',(-28.6378008601681,23.7500080620583,0.600000000000003));
#9326=CARTESIAN_POINT('',(-22.144476402432,17.2566836043221,0.600000000000001));
#9327=CARTESIAN_POINT('',(-28.7842474695749,24.1035614526515,0.600000000000003));
#9328=CARTESIAN_POINT('Origin',(-28.2842474695748,24.1035614526515,0.600000000000003));
#9329=CARTESIAN_POINT('',(-28.7842474695749,26.1117112172572,0.600000000000003));
#9330=CARTESIAN_POINT('',(-28.7842474695749,20.4294621680221,0.600000000000001));
#9331=CARTESIAN_POINT('',(-28.6463164350921,26.4565388034641,0.600000000000003));
#9332=CARTESIAN_POINT('Origin',(-28.2842474695748,26.1117112172572,0.600000000000003));
#9333=CARTESIAN_POINT('',(-26.7048541825725,28.4950741686097,0.600000000000003));
#9334=CARTESIAN_POINT('',(-26.4695350109151,28.74215929885,0.600000000000003));
#9335=CARTESIAN_POINT('',(-26.3427852170552,28.6502465824028,0.600000000000003));
#9336=CARTESIAN_POINT('Origin',(-26.3427852170552,28.1502465824028,0.600000000000003));
#9337=CARTESIAN_POINT('',(-4.84975341759722,28.6502465824028,0.600000000000003));
#9338=CARTESIAN_POINT('',(-8.16563247623254,28.6502465824028,0.600000000000003));
#9339=CARTESIAN_POINT('',(-1.34975341759722,25.1502465824028,0.600000000000003));
#9340=CARTESIAN_POINT('Origin',(-4.84975341759722,25.1502465824028,0.600000000000003));
#9341=CARTESIAN_POINT('',(-1.34975341759722,3.65721478294477,0.600000000000001));
#9342=CARTESIAN_POINT('',(-1.34975341759722,19.7487298505949,0.600000000000001));
#9343=CARTESIAN_POINT('Origin',(-1.84975341759722,3.65721478294477,0.600000000000001));
#9344=CARTESIAN_POINT('',(-10.8648573190427,23.3513464861378,0.600000000000003));
#9345=CARTESIAN_POINT('Origin',(-10.8648573190427,25.1013464861379,0.600000000000003));
#9346=CARTESIAN_POINT('',(-6.64865351386214,11.2651426809573,0.600000000000001));
#9347=CARTESIAN_POINT('Origin',(-4.89865351386214,11.2651426809573,0.600000000000001));
#9348=CARTESIAN_POINT('',(-20.801482994706,15.198517005294,0.600000000000001));
#9349=CARTESIAN_POINT('Origin',(-14.801482994706,15.198517005294,0.600000000000001));
#9350=CARTESIAN_POINT('',(-6.64865351386214,19.1351426809573,0.600000000000001));
#9351=CARTESIAN_POINT('Origin',(-4.89865351386214,19.1351426809573,0.600000000000001));
#9352=CARTESIAN_POINT('Origin',(-10.8648573190427,25.1013464861379,0.850000000000002));
#9353=CARTESIAN_POINT('',(-10.8648573190427,23.6013464861379,0.850000000000002));
#9354=CARTESIAN_POINT('Origin',(-4.89865351386214,19.1351426809573,0.85));
#9355=CARTESIAN_POINT('',(-6.39865351386215,19.1351426809573,0.85));
#9356=CARTESIAN_POINT('Origin',(-4.89865351386214,11.2651426809573,0.85));
#9357=CARTESIAN_POINT('',(-6.39865351386215,11.2651426809573,0.85));
#9358=CARTESIAN_POINT('Origin',(-1.03334796495904,3.39902949974303,0.85));
#9359=CARTESIAN_POINT('',(-3.19863361032902,0.99161459939066,1.1));
#9360=CARTESIAN_POINT('',(-3.19863361032902,0.99161459939066,1.1));
#9361=CARTESIAN_POINT('',(-1.16009824518343,2.93307685191027,1.1));
#9362=CARTESIAN_POINT('',(-1.50492583139032,3.29514581742752,0.600000000000001));
#9363=CARTESIAN_POINT('',(-0.860934171855591,3.21799501698441,1.1));
#9364=CARTESIAN_POINT('Origin',(-3.88828878274281,1.71575253042515,0.849999999999997));
#9365=CARTESIAN_POINT('',(-3.88828878274281,0.715752530425142,1.1));
#9366=CARTESIAN_POINT('Origin',(-3.88828878274281,1.71575253042514,1.1));
#9367=CARTESIAN_POINT('',(-3.88828878274281,0.715752530425142,1.1));
#9368=CARTESIAN_POINT('Origin',(-7.48490015880533,0.96575253042515,0.849999999999997));
#9369=CARTESIAN_POINT('',(-5.89643854734845,0.715752530425142,1.1));
#9370=CARTESIAN_POINT('',(-5.89643854734845,0.715752530425142,1.1));
#9371=CARTESIAN_POINT('',(-7.48490015880533,0.715752530425142,1.1));
#9372=CARTESIAN_POINT('Origin',(-5.89643854734845,1.71575253042515,0.849999999999997));
#9373=CARTESIAN_POINT('',(-6.603545328535,1.00864574923859,1.1));
#9374=CARTESIAN_POINT('Origin',(-5.89643854734845,1.71575253042514,1.1));
#9375=CARTESIAN_POINT('',(-6.603545328535,1.00864574923859,1.1));
#9376=CARTESIAN_POINT('Origin',(-10.834455417802,5.59310922909884,0.85));
#9377=CARTESIAN_POINT('',(-8.68678411623867,3.09188453694227,1.1));
#9378=CARTESIAN_POINT('',(-8.68678411623867,3.09188453694227,1.1));
#9379=CARTESIAN_POINT('',(-11.0112321130986,5.4163325338022,1.1));
#9380=CARTESIAN_POINT('Origin',(-7.97967733505213,3.79899131812882,0.85));
#9381=CARTESIAN_POINT('',(-8.97967733505213,3.79899131812881,1.1));
#9382=CARTESIAN_POINT('Origin',(-7.97967733505213,3.79899131812881,1.1));
#9383=CARTESIAN_POINT('',(-8.97967733505213,3.79899131812881,1.1));
#9384=CARTESIAN_POINT('Origin',(-8.72967733505213,8.86599543727139,0.85));
#9385=CARTESIAN_POINT('',(-8.97967733505212,5.32126156243407,1.1));
#9386=CARTESIAN_POINT('',(-8.97967733505212,5.32126156243407,1.1));
#9387=CARTESIAN_POINT('',(-8.97967733505213,8.86599543727138,1.1));
#9388=CARTESIAN_POINT('Origin',(-10.9796773350521,5.32126156243408,0.85));
#9389=CARTESIAN_POINT('',(-12.6152248047351,6.47234126185272,1.1));
#9390=CARTESIAN_POINT('',(-12.6152248047351,6.47234126185272,1.1));
#9391=CARTESIAN_POINT('Origin',(-10.9796773350521,5.32126156243407,1.1));
#9392=CARTESIAN_POINT('Origin',(-13.4329985395765,7.04788111156204,0.85));
#9393=CARTESIAN_POINT('',(-13.4329985395765,6.04788111156203,1.1));
#9394=CARTESIAN_POINT('Origin',(-13.4329985395765,7.04788111156204,1.1));
#9395=CARTESIAN_POINT('',(-13.4329985395765,6.04788111156203,1.1));
#9396=CARTESIAN_POINT('Origin',(-12.1622628350393,6.29788111156204,0.85));
#9397=CARTESIAN_POINT('',(-19.8602068534659,6.04788111156203,1.1));
#9398=CARTESIAN_POINT('',(-19.8602068534659,6.04788111156203,1.1));
#9399=CARTESIAN_POINT('',(-12.1622628350393,6.04788111156203,1.1));
#9400=CARTESIAN_POINT('Origin',(-19.8602068534659,7.04788111156204,0.85));
#9401=CARTESIAN_POINT('',(-20.5673136346525,6.34077433037548,1.1));
#9402=CARTESIAN_POINT('Origin',(-19.8602068534659,7.04788111156203,1.1));
#9403=CARTESIAN_POINT('',(-20.5673136346525,6.34077433037548,1.1));
#9404=CARTESIAN_POINT('Origin',(-19.9742495021059,6.10126358842215,0.85));
#9405=CARTESIAN_POINT('',(-23.6592256696245,9.43268636534752,1.1));
#9406=CARTESIAN_POINT('',(-23.6592256696245,9.43268636534752,1.1));
#9407=CARTESIAN_POINT('',(-20.1510261974025,5.9244868931255,1.1));
#9408=CARTESIAN_POINT('Origin',(-22.952118888438,10.1397931465341,0.85));
#9409=CARTESIAN_POINT('',(-23.952118888438,10.1397931465341,1.1));
#9410=CARTESIAN_POINT('Origin',(-22.952118888438,10.1397931465341,1.1));
#9411=CARTESIAN_POINT('',(-23.952118888438,10.1397931465341,1.1));
#9412=CARTESIAN_POINT('Origin',(-23.702118888438,15.7520994917882,0.85));
#9413=CARTESIAN_POINT('',(-23.952118888438,16.5670014604234,1.1));
#9414=CARTESIAN_POINT('',(-23.952118888438,15.7520994917882,1.1));
#9415=CARTESIAN_POINT('',(-23.952118888438,16.5670014604234,1.1));
#9416=CARTESIAN_POINT('Origin',(-22.952118888438,16.5670014604234,0.85));
#9417=CARTESIAN_POINT('',(-23.5276587381473,17.3847751952649,1.1));
#9418=CARTESIAN_POINT('Origin',(-22.952118888438,16.5670014604234,1.1));
#9419=CARTESIAN_POINT('',(-23.5276587381473,17.3847751952649,1.1));
#9420=CARTESIAN_POINT('Origin',(-24.6787384375659,19.0203226649479,0.85));
#9421=CARTESIAN_POINT('',(-24.6787384375659,21.0203226649479,1.10000000000001));
#9422=CARTESIAN_POINT('Origin',(-24.6787384375659,19.0203226649479,1.1));
#9423=CARTESIAN_POINT('',(-24.6787384375659,21.0203226649479,1.10000000000001));
#9424=CARTESIAN_POINT('Origin',(-19.0483668895561,21.2703226649479,0.850000000000002));
#9425=CARTESIAN_POINT('',(-26.2010086818712,21.0203226649479,1.10000000000001));
#9426=CARTESIAN_POINT('',(-19.0483668895561,21.0203226649479,1.10000000000001));
#9427=CARTESIAN_POINT('',(-26.2010086818712,21.0203226649479,1.10000000000001));
#9428=CARTESIAN_POINT('Origin',(-26.2010086818712,22.0203226649479,0.850000000000002));
#9429=CARTESIAN_POINT('',(-26.9081154630577,21.3132158837613,1.10000000000001));
#9430=CARTESIAN_POINT('Origin',(-26.2010086818712,22.0203226649479,1.1));
#9431=CARTESIAN_POINT('',(-26.9081154630577,21.3132158837613,1.10000000000001));
#9432=CARTESIAN_POINT('Origin',(-22.3212530977286,17.0799069090255,0.850000000000002));
#9433=CARTESIAN_POINT('',(-28.9913542507614,23.396454671465,1.10000000000001));
#9434=CARTESIAN_POINT('',(-22.4980297930252,16.9031302137289,1.1));
#9435=CARTESIAN_POINT('',(-28.9913542507614,23.396454671465,1.10000000000001));
#9436=CARTESIAN_POINT('Origin',(-28.2842474695748,24.1035614526515,0.850000000000002));
#9437=CARTESIAN_POINT('',(-29.2842474695749,24.1035614526515,1.1));
#9438=CARTESIAN_POINT('Origin',(-28.2842474695748,24.1035614526515,1.1));
#9439=CARTESIAN_POINT('',(-29.2842474695749,24.1035614526515,1.1));
#9440=CARTESIAN_POINT('Origin',(-29.0342474695749,20.4294621680221,0.85));
#9441=CARTESIAN_POINT('',(-29.2842474695749,26.1117112172572,1.1));
#9442=CARTESIAN_POINT('',(-29.2842474695749,20.4294621680221,1.1));
#9443=CARTESIAN_POINT('',(-29.2842474695749,26.1117112172572,1.1));
#9444=CARTESIAN_POINT('Origin',(-28.2842474695748,26.1117112172572,0.850000000000002));
#9445=CARTESIAN_POINT('',(-29.0083854006093,26.801366389671,1.1));
#9446=CARTESIAN_POINT('Origin',(-28.2842474695748,26.1117112172572,1.1));
#9447=CARTESIAN_POINT('',(-29.0083854006093,26.801366389671,1.1));
#9448=CARTESIAN_POINT('Origin',(-26.6505694936737,28.9145730919534,0.850000000000002));
#9449=CARTESIAN_POINT('',(-27.0669231480897,28.8399017548166,1.1));
#9450=CARTESIAN_POINT('',(-26.8316039764323,29.0869868850569,1.1));
#9451=CARTESIAN_POINT('',(-27.0669231480897,28.8399017548166,1.1));
#9452=CARTESIAN_POINT('Origin',(-26.3427852170552,28.1502465824028,0.850000000000002));
#9453=CARTESIAN_POINT('',(-26.3427852170552,29.1502465824028,1.1));
#9454=CARTESIAN_POINT('Origin',(-26.3427852170552,28.1502465824028,1.1));
#9455=CARTESIAN_POINT('',(-26.3427852170552,29.1502465824028,1.1));
#9456=CARTESIAN_POINT('Origin',(-8.16563247623254,28.9002465824028,0.850000000000002));
#9457=CARTESIAN_POINT('',(-4.84975341759722,29.1502465824028,1.1));
#9458=CARTESIAN_POINT('',(-8.16563247623254,29.1502465824028,1.1));
#9459=CARTESIAN_POINT('',(-4.84975341759722,29.1502465824028,1.1));
#9460=CARTESIAN_POINT('Origin',(-4.84975341759722,25.1502465824028,0.850000000000002));
#9461=CARTESIAN_POINT('',(-0.849753417597219,25.1502465824028,1.1));
#9462=CARTESIAN_POINT('Origin',(-4.84975341759722,25.1502465824028,1.1));
#9463=CARTESIAN_POINT('',(-0.849753417597219,25.1502465824028,1.1));
#9464=CARTESIAN_POINT('Origin',(-1.09975341759722,19.7487298505949,0.85));
#9465=CARTESIAN_POINT('',(-0.849753417597219,3.65721478294476,1.1));
#9466=CARTESIAN_POINT('',(-0.849753417597219,3.65721478294476,1.1));
#9467=CARTESIAN_POINT('',(-0.849753417597219,19.7487298505949,1.1));
#9468=CARTESIAN_POINT('Origin',(-1.84975341759722,3.65721478294477,0.85));
#9469=CARTESIAN_POINT('Origin',(-1.84975341759722,3.65721478294476,1.1));
#9470=CARTESIAN_POINT('Origin',(-23.952118888438,17.1569858647893,19.));
#9471=CARTESIAN_POINT('',(-23.952118888438,10.1397931465341,7.2));
#9472=CARTESIAN_POINT('',(-23.952118888438,10.1397931465341,19.));
#9473=CARTESIAN_POINT('',(-23.952118888438,16.5670014604234,7.2));
#9474=CARTESIAN_POINT('',(-23.952118888438,15.7520994917882,7.2));
#9475=CARTESIAN_POINT('',(-23.952118888438,16.5670014604234,19.));
#9476=CARTESIAN_POINT('Origin',(-22.952118888438,10.1397931465341,19.));
#9477=CARTESIAN_POINT('',(-23.6592256696245,9.43268636534752,7.2));
#9478=CARTESIAN_POINT('',(-23.6592256696245,9.43268636534752,19.));
#9479=CARTESIAN_POINT('Origin',(-22.952118888438,10.1397931465341,7.2));
#9480=CARTESIAN_POINT('Origin',(-20.274420415839,6.04788111156204,19.));
#9481=CARTESIAN_POINT('',(-20.5673136346525,6.34077433037548,7.2));
#9482=CARTESIAN_POINT('',(-20.5673136346525,6.34077433037549,19.));
#9483=CARTESIAN_POINT('',(-20.1510261974025,5.9244868931255,7.2));
#9484=CARTESIAN_POINT('Origin',(-19.8602068534659,7.04788111156204,19.));
#9485=CARTESIAN_POINT('',(-19.8602068534659,6.04788111156203,7.2));
#9486=CARTESIAN_POINT('',(-19.8602068534659,6.04788111156204,19.));
#9487=CARTESIAN_POINT('Origin',(-19.8602068534659,7.04788111156203,7.2));
#9488=CARTESIAN_POINT('Origin',(-12.8430141352107,6.04788111156204,19.));
#9489=CARTESIAN_POINT('',(-13.4329985395765,6.04788111156203,7.2));
#9490=CARTESIAN_POINT('',(-13.4329985395765,6.04788111156204,19.));
#9491=CARTESIAN_POINT('',(-12.1622628350393,6.04788111156203,7.2));
#9492=CARTESIAN_POINT('Origin',(-13.4329985395765,7.04788111156204,19.));
#9493=CARTESIAN_POINT('',(-12.6152248047351,6.47234126185272,7.2));
#9494=CARTESIAN_POINT('',(-12.6152248047351,6.47234126185272,19.));
#9495=CARTESIAN_POINT('Origin',(-13.4329985395765,7.04788111156204,7.2));
#9496=CARTESIAN_POINT('Origin',(-10.9796773350521,5.32126156243408,19.));
#9497=CARTESIAN_POINT('',(-8.97967733505212,5.32126156243407,7.2));
#9498=CARTESIAN_POINT('',(-8.97967733505212,5.32126156243408,19.));
#9499=CARTESIAN_POINT('Origin',(-10.9796773350521,5.32126156243407,7.2));
#9500=CARTESIAN_POINT('Origin',(-8.97967733505213,3.38477775575572,19.));
#9501=CARTESIAN_POINT('',(-8.97967733505213,3.79899131812881,7.2));
#9502=CARTESIAN_POINT('',(-8.97967733505213,3.79899131812882,19.));
#9503=CARTESIAN_POINT('',(-8.97967733505213,8.86599543727138,7.2));
#9504=CARTESIAN_POINT('Origin',(-7.97967733505213,3.79899131812882,19.));
#9505=CARTESIAN_POINT('',(-8.68678411623867,3.09188453694227,7.2));
#9506=CARTESIAN_POINT('',(-8.68678411623867,3.09188453694227,19.));
#9507=CARTESIAN_POINT('Origin',(-7.97967733505213,3.79899131812881,7.2));
#9508=CARTESIAN_POINT('Origin',(-6.31065210972155,0.715752530425147,19.));
#9509=CARTESIAN_POINT('',(-6.603545328535,1.00864574923859,7.2));
#9510=CARTESIAN_POINT('',(-6.603545328535,1.0086457492386,19.));
#9511=CARTESIAN_POINT('',(-11.0112321130986,5.4163325338022,7.2));
#9512=CARTESIAN_POINT('Origin',(-5.89643854734845,1.71575253042514,19.));
#9513=CARTESIAN_POINT('',(-5.89643854734845,0.715752530425142,7.2));
#9514=CARTESIAN_POINT('',(-5.89643854734845,0.715752530425147,19.));
#9515=CARTESIAN_POINT('Origin',(-5.89643854734845,1.71575253042514,7.2));
#9516=CARTESIAN_POINT('Origin',(-3.48828878274281,0.715752530425147,19.));
#9517=CARTESIAN_POINT('',(-3.88828878274281,0.715752530425142,7.2));
#9518=CARTESIAN_POINT('',(-3.88828878274281,0.715752530425147,19.));
#9519=CARTESIAN_POINT('',(-7.48490015880533,0.715752530425142,7.2));
#9520=CARTESIAN_POINT('Origin',(-3.88828878274281,1.71575253042515,19.));
#9521=CARTESIAN_POINT('',(-3.19863361032902,0.99161459939066,7.2));
#9522=CARTESIAN_POINT('',(-3.19863361032902,0.991614599390664,19.));
#9523=CARTESIAN_POINT('Origin',(-3.88828878274281,1.71575253042514,7.2));
#9524=CARTESIAN_POINT('Origin',(-0.849753417597219,3.22864335437334,19.));
#9525=CARTESIAN_POINT('',(-1.16009824518343,2.93307685191027,7.2));
#9526=CARTESIAN_POINT('',(-1.16009824518343,2.93307685191028,19.));
#9527=CARTESIAN_POINT('',(-0.860934171855592,3.21799501698441,7.2));
#9528=CARTESIAN_POINT('Origin',(-1.03334796495904,3.39902949974302,7.45));
#9529=CARTESIAN_POINT('',(-3.54346119653592,1.3536835649079,7.69999999999999));
#9530=CARTESIAN_POINT('',(-1.16009824518343,2.93307685191027,7.2));
#9531=CARTESIAN_POINT('Origin',(-3.88828878274281,1.71575253042514,7.44999999999999));
#9532=CARTESIAN_POINT('',(-3.88828878274281,1.21575253042514,7.69999999999999));
#9533=CARTESIAN_POINT('Origin',(-7.48490015880533,0.965752530425141,7.44999999999999));
#9534=CARTESIAN_POINT('',(-5.89643854734845,1.21575253042514,7.69999999999999));
#9535=CARTESIAN_POINT('Origin',(-5.89643854734845,1.71575253042514,7.44999999999999));
#9536=CARTESIAN_POINT('',(-6.24999193794173,1.36219913983186,7.69999999999999));
#9537=CARTESIAN_POINT('Origin',(-10.834455417802,5.59310922909884,7.45));
#9538=CARTESIAN_POINT('',(-8.3332307256454,3.44543792753554,7.7));
#9539=CARTESIAN_POINT('Origin',(-7.97967733505213,3.79899131812881,7.45));
#9540=CARTESIAN_POINT('',(-8.47967733505213,3.79899131812881,7.7));
#9541=CARTESIAN_POINT('Origin',(-8.72967733505213,8.86599543727138,7.45));
#9542=CARTESIAN_POINT('',(-8.47967733505213,5.32126156243407,7.7));
#9543=CARTESIAN_POINT('Origin',(-10.9796773350521,5.32126156243407,7.45));
#9544=CARTESIAN_POINT('',(-13.0241116721558,6.76011118670738,7.7));
#9545=CARTESIAN_POINT('Origin',(-13.4329985395765,7.04788111156204,7.45));
#9546=CARTESIAN_POINT('',(-13.4329985395765,6.54788111156204,7.7));
#9547=CARTESIAN_POINT('Origin',(-12.1622628350393,6.29788111156203,7.45));
#9548=CARTESIAN_POINT('',(-19.8602068534659,6.54788111156203,7.7));
#9549=CARTESIAN_POINT('Origin',(-19.8602068534659,7.04788111156203,7.45));
#9550=CARTESIAN_POINT('',(-20.2137602440592,6.69432772096875,7.7));
#9551=CARTESIAN_POINT('Origin',(-19.9742495021059,6.10126358842214,7.45));
#9552=CARTESIAN_POINT('',(-23.3056722790312,9.78623975594079,7.7));
#9553=CARTESIAN_POINT('Origin',(-22.952118888438,10.1397931465341,7.45));
#9554=CARTESIAN_POINT('',(-23.452118888438,10.1397931465341,7.7));
#9555=CARTESIAN_POINT('Origin',(-23.702118888438,15.7520994917882,7.45));
#9556=CARTESIAN_POINT('',(-23.452118888438,16.5670014604234,7.7));
#9557=CARTESIAN_POINT('Origin',(-22.952118888438,16.5670014604234,7.45));
#9558=CARTESIAN_POINT('',(-23.5276587381473,17.3847751952649,7.2));
#9559=CARTESIAN_POINT('',(-23.2398888132926,16.9758883278442,7.7));
#9560=CARTESIAN_POINT('Origin',(-22.952118888438,16.5670014604234,7.2));
#9561=CARTESIAN_POINT('Origin',(-24.6787384375659,19.0203226649479,7.45));
#9562=CARTESIAN_POINT('',(-24.6787384375659,21.0203226649479,7.2));
#9563=CARTESIAN_POINT('',(-24.6787384375659,21.5203226649479,7.7));
#9564=CARTESIAN_POINT('Origin',(-24.6787384375659,19.0203226649479,7.2));
#9565=CARTESIAN_POINT('Origin',(-19.0483668895561,21.2703226649479,7.45));
#9566=CARTESIAN_POINT('',(-26.2010086818712,21.0203226649479,7.2));
#9567=CARTESIAN_POINT('',(-26.2010086818712,21.5203226649479,7.7));
#9568=CARTESIAN_POINT('',(-19.0483668895561,21.0203226649479,7.2));
#9569=CARTESIAN_POINT('Origin',(-26.2010086818712,22.0203226649479,7.45));
#9570=CARTESIAN_POINT('',(-26.9081154630577,21.3132158837613,7.2));
#9571=CARTESIAN_POINT('',(-26.5545620724644,21.6667692743546,7.7));
#9572=CARTESIAN_POINT('Origin',(-26.2010086818712,22.0203226649479,7.2));
#9573=CARTESIAN_POINT('Origin',(-22.3212530977286,17.0799069090255,7.45));
#9574=CARTESIAN_POINT('',(-28.9913542507614,23.396454671465,7.2));
#9575=CARTESIAN_POINT('',(-28.6378008601681,23.7500080620583,7.7));
#9576=CARTESIAN_POINT('',(-22.4980297930252,16.9031302137289,7.2));
#9577=CARTESIAN_POINT('Origin',(-28.2842474695748,24.1035614526515,7.45));
#9578=CARTESIAN_POINT('',(-29.2842474695749,24.1035614526515,7.2));
#9579=CARTESIAN_POINT('',(-28.7842474695749,24.1035614526515,7.7));
#9580=CARTESIAN_POINT('Origin',(-28.2842474695748,24.1035614526515,7.2));
#9581=CARTESIAN_POINT('Origin',(-29.0342474695749,20.4294621680221,7.45));
#9582=CARTESIAN_POINT('',(-29.2842474695749,26.1117112172572,7.2));
#9583=CARTESIAN_POINT('',(-28.7842474695749,26.1117112172572,7.7));
#9584=CARTESIAN_POINT('',(-29.2842474695749,20.4294621680221,7.2));
#9585=CARTESIAN_POINT('Origin',(-28.2842474695748,26.1117112172572,7.45));
#9586=CARTESIAN_POINT('',(-29.0083854006093,26.801366389671,7.2));
#9587=CARTESIAN_POINT('',(-28.6463164350921,26.4565388034641,7.7));
#9588=CARTESIAN_POINT('Origin',(-28.2842474695748,26.1117112172572,7.2));
#9589=CARTESIAN_POINT('Origin',(-26.6505694936737,28.9145730919534,7.45));
#9590=CARTESIAN_POINT('',(-27.0669231480897,28.8399017548166,7.2));
#9591=CARTESIAN_POINT('',(-26.7048541825725,28.4950741686097,7.7));
#9592=CARTESIAN_POINT('',(-26.8316039764323,29.0869868850569,7.2));
#9593=CARTESIAN_POINT('Origin',(-26.3427852170552,28.1502465824028,7.45));
#9594=CARTESIAN_POINT('',(-26.3427852170552,29.1502465824028,7.2));
#9595=CARTESIAN_POINT('',(-26.3427852170552,28.6502465824028,7.7));
#9596=CARTESIAN_POINT('Origin',(-26.3427852170552,28.1502465824028,7.2));
#9597=CARTESIAN_POINT('Origin',(-8.16563247623254,28.9002465824028,7.45));
#9598=CARTESIAN_POINT('',(-4.84975341759722,29.1502465824028,7.2));
#9599=CARTESIAN_POINT('',(-4.84975341759722,28.6502465824028,7.7));
#9600=CARTESIAN_POINT('',(-8.16563247623254,29.1502465824028,7.2));
#9601=CARTESIAN_POINT('Origin',(-4.84975341759722,25.1502465824028,7.45));
#9602=CARTESIAN_POINT('',(-0.849753417597219,25.1502465824028,7.2));
#9603=CARTESIAN_POINT('',(-1.34975341759722,25.1502465824028,7.7));
#9604=CARTESIAN_POINT('Origin',(-4.84975341759722,25.1502465824028,7.2));
#9605=CARTESIAN_POINT('Origin',(-1.09975341759722,19.7487298505949,7.45));
#9606=CARTESIAN_POINT('',(-0.849753417597219,3.65721478294476,7.2));
#9607=CARTESIAN_POINT('',(-1.34975341759722,3.65721478294476,7.7));
#9608=CARTESIAN_POINT('',(-0.849753417597219,19.7487298505949,7.2));
#9609=CARTESIAN_POINT('Origin',(-1.84975341759722,3.65721478294476,7.45));
#9610=CARTESIAN_POINT('Origin',(-1.84975341759722,3.65721478294476,7.2));
#9611=CARTESIAN_POINT('Origin',(-24.6787384375659,19.0203226649479,19.));
#9612=CARTESIAN_POINT('',(-23.5276587381473,17.3847751952649,19.));
#9613=CARTESIAN_POINT('',(-24.6787384375659,21.0203226649479,19.));
#9614=CARTESIAN_POINT('Origin',(-26.6152222442443,21.0203226649479,19.));
#9615=CARTESIAN_POINT('',(-26.2010086818712,21.0203226649479,19.));
#9616=CARTESIAN_POINT('Origin',(-26.2010086818712,22.0203226649479,19.));
#9617=CARTESIAN_POINT('',(-26.9081154630577,21.3132158837613,19.));
#9618=CARTESIAN_POINT('Origin',(-29.2842474695749,23.6893478902784,19.));
#9619=CARTESIAN_POINT('',(-28.9913542507614,23.396454671465,19.));
#9620=CARTESIAN_POINT('Origin',(-28.2842474695748,24.1035614526515,19.));
#9621=CARTESIAN_POINT('',(-29.2842474695749,24.1035614526515,19.));
#9622=CARTESIAN_POINT('Origin',(-29.2842474695749,26.5117112172572,19.));
#9623=CARTESIAN_POINT('',(-29.2842474695749,26.1117112172572,19.));
#9624=CARTESIAN_POINT('Origin',(-28.2842474695748,26.1117112172572,19.));
#9625=CARTESIAN_POINT('',(-29.0083854006093,26.801366389671,19.));
#9626=CARTESIAN_POINT('Origin',(-26.7713566456267,29.1502465824028,19.));
#9627=CARTESIAN_POINT('',(-27.0669231480897,28.8399017548166,19.));
#9628=CARTESIAN_POINT('Origin',(-26.3427852170552,28.1502465824028,19.));
#9629=CARTESIAN_POINT('',(-26.3427852170552,29.1502465824028,19.));
#9630=CARTESIAN_POINT('Origin',(-4.84975341759722,29.1502465824028,19.));
#9631=CARTESIAN_POINT('',(-4.84975341759722,29.1502465824028,19.));
#9632=CARTESIAN_POINT('Origin',(-4.84975341759722,25.1502465824028,19.));
#9633=CARTESIAN_POINT('',(-0.849753417597219,25.1502465824028,19.));
#9634=CARTESIAN_POINT('Origin',(-0.849753417597219,25.1502465824028,19.));
#9635=CARTESIAN_POINT('',(-0.849753417597219,3.65721478294476,19.));
#9636=CARTESIAN_POINT('Origin',(-1.84975341759722,3.65721478294476,19.));
#9637=CARTESIAN_POINT('Origin',(-22.952118888438,16.5670014604234,19.));
#9638=CARTESIAN_POINT('Origin',(-14.801482994706,15.198517005294,19.));
#9639=CARTESIAN_POINT('',(-20.801482994706,15.198517005294,19.));
#9640=CARTESIAN_POINT('',(0.,0.,0.));
#9641=CARTESIAN_POINT('Origin',(-10.9359120418715,27.7504782148047,17.6));
#9642=CARTESIAN_POINT('',(-10.2859120418715,27.8004782148047,17.6));
#9643=CARTESIAN_POINT('Origin',(-10.9359120418715,27.8004782148047,17.6));
#9644=CARTESIAN_POINT('',(-10.1859120418715,27.7004782148047,17.6));
#9645=CARTESIAN_POINT('',(-10.2359120418715,27.7504782148047,17.6));
#9646=CARTESIAN_POINT('Origin',(-10.9359120418715,27.7004782148047,17.6));
#9647=CARTESIAN_POINT('Origin',(-10.9359120418715,22.4004782148047,17.6));
#9648=CARTESIAN_POINT('',(-10.1859120418715,22.5004782148047,17.6));
#9649=CARTESIAN_POINT('',(-10.1859120418715,22.4004782148047,17.6));
#9650=CARTESIAN_POINT('Origin',(-10.9359120418715,22.5004782148047,17.6));
#9651=CARTESIAN_POINT('Origin',(-10.9359120418715,27.8004782148047,17.6));
#9652=CARTESIAN_POINT('Origin',(-10.9359120418715,22.4504782148047,17.6));
#9653=CARTESIAN_POINT('',(-10.2859120418715,22.4004782148047,17.6));
#9654=CARTESIAN_POINT('',(-10.2359120418715,22.4504782148047,17.6));
#9655=CARTESIAN_POINT('Origin',(-10.9359120418715,22.4004782148047,17.6));
#9656=CARTESIAN_POINT('Origin',(-10.9359120418715,22.4004782148047,17.6));
#9657=CARTESIAN_POINT('',(0.,0.,0.));
#9658=CARTESIAN_POINT('Origin',(-4.88927830720691,5.31072169279307,9.2));
#9659=CARTESIAN_POINT('',(-7.48735451856022,5.31072169279307,7.7));
#9660=CARTESIAN_POINT('Origin',(-4.88927830720691,5.31072169279307,7.7));
#9661=CARTESIAN_POINT('',(-4.88927830720691,5.31072169279307,6.2));
#9662=CARTESIAN_POINT('Origin',(-4.88927830720691,5.31072169279307,9.2));
#9663=CARTESIAN_POINT('Origin',(-4.88927830720691,5.31072169279307,8.2));
#9664=CARTESIAN_POINT('',(-7.54689383586007,5.31072169279307,7.7));
#9665=CARTESIAN_POINT('Origin',(-4.88927830720691,5.31072169279307,7.7));
#9666=CARTESIAN_POINT('',(-8.04689383586007,5.31072169279307,8.2));
#9667=CARTESIAN_POINT('Origin',(-7.54689383586007,5.31072169279307,8.2));
#9668=CARTESIAN_POINT('Origin',(-4.88927830720691,5.31072169279307,8.2));
#9669=CARTESIAN_POINT('Origin',(-4.88927830720691,5.31072169279308,19.));
#9670=CARTESIAN_POINT('',(-8.04689383586007,5.31072169279308,18.5));
#9671=CARTESIAN_POINT('',(-8.04689383586007,5.31072169279308,19.));
#9672=CARTESIAN_POINT('Origin',(-4.88927830720691,5.31072169279308,18.5));
#9673=CARTESIAN_POINT('Origin',(-4.88927830720691,5.31072169279307,7.7));
#9674=CARTESIAN_POINT('Origin',(-4.88927830720691,3.5786708852242,19.));
#9675=CARTESIAN_POINT('',(-4.88927830720691,3.5786708852242,19.));
#9676=CARTESIAN_POINT('',(-6.38927830720691,4.44469628900864,19.));
#9677=CARTESIAN_POINT('',(-5.26427830720691,3.79517723617031,19.));
#9678=CARTESIAN_POINT('',(-4.88927830720691,3.5786708852242,18.));
#9679=CARTESIAN_POINT('',(-4.88927830720691,3.5786708852242,19.));
#9680=CARTESIAN_POINT('',(-6.38927830720691,4.44469628900864,18.));
#9681=CARTESIAN_POINT('',(-6.38927830720691,4.44469628900864,18.));
#9682=CARTESIAN_POINT('',(-6.38927830720691,4.44469628900864,19.));
#9683=CARTESIAN_POINT('Origin',(-3.38927830720691,4.44469628900864,19.));
#9684=CARTESIAN_POINT('',(-3.38927830720691,4.44469628900864,19.));
#9685=CARTESIAN_POINT('',(-3.76427830720691,4.22818993806253,19.));
#9686=CARTESIAN_POINT('',(-3.38927830720691,4.44469628900864,18.));
#9687=CARTESIAN_POINT('',(-3.38927830720691,4.44469628900864,19.));
#9688=CARTESIAN_POINT('',(-4.88927830720691,3.5786708852242,18.));
#9689=CARTESIAN_POINT('Origin',(-3.38927830720691,6.17674709657752,19.));
#9690=CARTESIAN_POINT('',(-3.38927830720691,6.17674709657752,19.));
#9691=CARTESIAN_POINT('',(-3.38927830720691,5.7437343946853,19.));
#9692=CARTESIAN_POINT('',(-3.38927830720691,6.17674709657751,18.));
#9693=CARTESIAN_POINT('',(-3.38927830720691,6.17674709657752,19.));
#9694=CARTESIAN_POINT('',(-3.38927830720691,4.44469628900864,18.));
#9695=CARTESIAN_POINT('Origin',(-4.88927830720691,7.04277250036196,19.));
#9696=CARTESIAN_POINT('',(-4.88927830720691,7.04277250036196,19.));
#9697=CARTESIAN_POINT('',(-4.51427830720691,6.82626614941585,19.));
#9698=CARTESIAN_POINT('',(-4.88927830720691,7.04277250036195,18.));
#9699=CARTESIAN_POINT('',(-4.88927830720691,7.04277250036196,19.));
#9700=CARTESIAN_POINT('',(-3.38927830720691,6.17674709657751,18.));
#9701=CARTESIAN_POINT('Origin',(-6.38927830720691,6.17674709657752,19.));
#9702=CARTESIAN_POINT('',(-6.38927830720691,6.17674709657752,19.));
#9703=CARTESIAN_POINT('',(-6.01427830720691,6.39325344752363,19.));
#9704=CARTESIAN_POINT('',(-6.38927830720691,6.17674709657751,18.));
#9705=CARTESIAN_POINT('',(-6.38927830720691,6.17674709657752,19.));
#9706=CARTESIAN_POINT('',(-4.88927830720691,7.04277250036195,18.));
#9707=CARTESIAN_POINT('Origin',(-6.38927830720691,4.44469628900864,19.));
#9708=CARTESIAN_POINT('',(-6.38927830720691,4.87770899090086,19.));
#9709=CARTESIAN_POINT('',(-6.38927830720691,6.17674709657751,18.));
#9710=CARTESIAN_POINT('Origin',(-4.88927830720691,5.31072169279307,18.));
#9711=CARTESIAN_POINT('Origin',(-4.88927830720691,5.31072169279308,18.75));
#9712=CARTESIAN_POINT('',(-7.54689383586007,5.31072169279308,19.));
#9713=CARTESIAN_POINT('Origin',(-4.88927830720691,5.31072169279308,19.));
#9714=CARTESIAN_POINT('',(-7.79689383586007,5.31072169279308,18.75));
#9715=CARTESIAN_POINT('Origin',(-4.88927830720691,5.31072169279308,19.));
#9716=CARTESIAN_POINT('',(0.,0.,0.));
#9717=CARTESIAN_POINT('Origin',(-10.9359120418715,26.3504782148047,17.6));
#9718=CARTESIAN_POINT('',(-10.9359120418715,26.3504782148047,18.35));
#9719=CARTESIAN_POINT('Origin',(-10.9359120418715,26.3504782148047,18.6));
#9720=CARTESIAN_POINT('Origin',(-10.9359120418715,26.3504782148047,17.6));
#9721=CARTESIAN_POINT('',(-10.9359120418715,26.6004782148047,16.6));
#9722=CARTESIAN_POINT('',(-10.9359120418715,26.1004782148047,16.6));
#9723=CARTESIAN_POINT('Origin',(-10.9359120418715,26.3504782148047,16.6));
#9724=CARTESIAN_POINT('Ctrl Pts',(-10.9359120418715,26.6004782148047,16.6));
#9725=CARTESIAN_POINT('Ctrl Pts',(-10.9402193353539,26.6004782148047,16.5977092724426));
#9726=CARTESIAN_POINT('Ctrl Pts',(-10.9445589464746,26.6004467587024,16.5954788663774));
#9727=CARTESIAN_POINT('Ctrl Pts',(-10.9872540124717,26.5998563522904,16.5742560748851));
#9728=CARTESIAN_POINT('Ctrl Pts',(-11.0283064246552,26.5971771315259,16.559542959919));
#9729=CARTESIAN_POINT('Ctrl Pts',(-11.0701108612612,26.5930900009076,16.5481972195909));
#9730=CARTESIAN_POINT('Ctrl Pts',(-11.0708339684841,26.5930188703742,16.5480020646239));
#9731=CARTESIAN_POINT('Ctrl Pts',(-11.0827759229911,26.5918370097103,16.544797109728));
#9732=CARTESIAN_POINT('Ctrl Pts',(-11.094063293504,26.590615824153,16.5420298581508));
#9733=CARTESIAN_POINT('Ctrl Pts',(-11.110070277255,26.5887362807543,16.5384418503857));
#9734=CARTESIAN_POINT('Ctrl Pts',(-11.1147727349573,26.5881661562854,16.5374286265409));
#9735=CARTESIAN_POINT('Ctrl Pts',(-11.1230847074372,26.5871263380585,16.5357072275207));
#9736=CARTESIAN_POINT('Ctrl Pts',(-11.1266932353496,26.5866642710644,16.5349829852478));
#9737=CARTESIAN_POINT('Ctrl Pts',(-11.1343464784642,26.585661455081,16.5334946079531));
#9738=CARTESIAN_POINT('Ctrl Pts',(-11.1383928290144,26.5851177664648,16.5327358435474));
#9739=CARTESIAN_POINT('Ctrl Pts',(-11.1481733797635,26.5837704893605,16.5309679692519));
#9740=CARTESIAN_POINT('Ctrl Pts',(-11.1539124540547,26.5829524731398,16.5299854641958));
#9741=CARTESIAN_POINT('Ctrl Pts',(-11.1737387918633,26.5800291593595,16.5267739133408));
#9742=CARTESIAN_POINT('Ctrl Pts',(-11.1878669666236,26.577776425181,16.5248034466825));
#9743=CARTESIAN_POINT('Ctrl Pts',(-11.2400872187947,26.568769854808,16.5186110231589));
#9744=CARTESIAN_POINT('Ctrl Pts',(-11.2785053382042,26.5608013780416,16.5162061142361));
#9745=CARTESIAN_POINT('Ctrl Pts',(-11.3413563804704,26.5448431161272,16.5154725363415));
#9746=CARTESIAN_POINT('Ctrl Pts',(-11.3663341463412,26.5377137973801,16.5160451884648));
#9747=CARTESIAN_POINT('Ctrl Pts',(-11.4675067236831,26.5048705240401,16.5219235534991));
#9748=CARTESIAN_POINT('Ctrl Pts',(-11.5339527175624,26.4736908333921,16.5341985199053));
#9749=CARTESIAN_POINT('Ctrl Pts',(-11.6275973319121,26.408664050569,16.5639151059098));
#9750=CARTESIAN_POINT('Ctrl Pts',(-11.6584745098273,26.3779628401158,16.5791986989673));
#9751=CARTESIAN_POINT('Ctrl Pts',(-11.693043062557,26.3250017138209,16.605627659773));
#9752=CARTESIAN_POINT('Ctrl Pts',(-11.7019011653722,26.3029596082007,16.6166575639151));
#9753=CARTESIAN_POINT('Ctrl Pts',(-11.7077448592175,26.2652062478922,16.6350648852536));
#9754=CARTESIAN_POINT('Ctrl Pts',(-11.7070741798815,26.2486012355755,16.6429988757827));
#9755=CARTESIAN_POINT('Ctrl Pts',(-11.698268450351,26.2180039204305,16.6569651923278));
#9756=CARTESIAN_POINT('Ctrl Pts',(-11.6911945436197,26.2046479601392,16.6627780404676));
#9757=CARTESIAN_POINT('Ctrl Pts',(-11.6706730422176,26.1789460999401,16.6732083185761));
#9758=CARTESIAN_POINT('Ctrl Pts',(-11.6571316130369,26.1675135294197,16.677362768157));
#9759=CARTESIAN_POINT('Ctrl Pts',(-11.6199753453774,26.1438724951594,16.6848437491615));
#9760=CARTESIAN_POINT('Ctrl Pts',(-11.5946921404572,26.1337519058654,16.686910649375));
#9761=CARTESIAN_POINT('Ctrl Pts',(-11.5217072854985,26.1124320719796,16.6888104810606));
#9762=CARTESIAN_POINT('Ctrl Pts',(-11.4671883817412,26.1060347853434,16.6853604690573));
#9763=CARTESIAN_POINT('Ctrl Pts',(-11.2981182229277,26.0969290280957,16.6690502405298));
#9764=CARTESIAN_POINT('Ctrl Pts',(-11.0857203861473,26.1008383327785,16.6427595546923));
#9765=CARTESIAN_POINT('Ctrl Pts',(-10.941103632581,26.1004816814786,16.6015112866721));
#9766=CARTESIAN_POINT('Ctrl Pts',(-10.9385065750259,26.1004782148047,16.6007604391535));
#9767=CARTESIAN_POINT('Ctrl Pts',(-10.9359120418715,26.1004782148047,16.6));
#9768=CARTESIAN_POINT('Ctrl Pts',(-10.9359120418715,26.1004782148047,16.6));
#9769=CARTESIAN_POINT('Ctrl Pts',(-11.099536659246,26.1004782148047,16.553125));
#9770=CARTESIAN_POINT('Ctrl Pts',(-11.425478146952,26.0179944258633,16.459375));
#9771=CARTESIAN_POINT('Ctrl Pts',(-11.9300789153048,25.5673438360005,16.271875));
#9772=CARTESIAN_POINT('Ctrl Pts',(-12.0229540626903,24.6519632977172,16.0375));
#9773=CARTESIAN_POINT('Ctrl Pts',(-11.164885722509,23.9466553694149,15.75625));
#9774=CARTESIAN_POINT('Ctrl Pts',(-10.1047480288197,24.2694595959893,15.475));
#9775=CARTESIAN_POINT('Ctrl Pts',(-9.7826825635668,25.329679981508,15.19375));
#9776=CARTESIAN_POINT('Ctrl Pts',(-10.4860312388173,26.1867889046978,14.9125));
#9777=CARTESIAN_POINT('Ctrl Pts',(-11.5890842776128,26.0780137287588,14.63125));
#9778=CARTESIAN_POINT('Ctrl Pts',(-12.1116466665383,25.1004991337717,14.35));
#9779=CARTESIAN_POINT('Ctrl Pts',(-11.5891025224479,24.1228902184961,14.06875));
#9780=CARTESIAN_POINT('Ctrl Pts',(-10.4859854650458,24.0142573573597,13.7875));
#9781=CARTESIAN_POINT('Ctrl Pts',(-9.78277916381912,24.8711035465199,13.50625));
#9782=CARTESIAN_POINT('Ctrl Pts',(-10.1045513655818,25.9318409055902,13.225));
#9783=CARTESIAN_POINT('Ctrl Pts',(-11.1652837785312,26.2536089704377,12.94375));
#9784=CARTESIAN_POINT('Ctrl Pts',(-12.0221382397948,25.5504081019422,12.6625));
#9785=CARTESIAN_POINT('Ctrl Pts',(-11.9134895714075,24.4472815516099,12.38125));
#9786=CARTESIAN_POINT('Ctrl Pts',(-10.9359120418715,23.9247557910194,12.1));
#9787=CARTESIAN_POINT('Ctrl Pts',(-9.95833451233548,24.4472815516099,11.81875));
#9788=CARTESIAN_POINT('Ctrl Pts',(-9.84968584394817,25.5504081019422,11.5375));
#9789=CARTESIAN_POINT('Ctrl Pts',(-10.7065403052118,26.2536089704376,11.25625));
#9790=CARTESIAN_POINT('Ctrl Pts',(-11.7672727181612,25.9318409055902,10.975));
#9791=CARTESIAN_POINT('Ctrl Pts',(-12.0890449199239,24.8711035465198,10.69375));
#9792=CARTESIAN_POINT('Ctrl Pts',(-11.3858386186972,24.0142573573597,10.4125));
#9793=CARTESIAN_POINT('Ctrl Pts',(-10.2827215612951,24.1228902184961,10.13125));
#9794=CARTESIAN_POINT('Ctrl Pts',(-9.76017741720471,25.1004991337717,9.85000000000001));
#9795=CARTESIAN_POINT('Ctrl Pts',(-10.2827398061301,26.0780137287587,9.56874999999999));
#9796=CARTESIAN_POINT('Ctrl Pts',(-11.3857928449257,26.1867889046978,9.28750000000001));
#9797=CARTESIAN_POINT('Ctrl Pts',(-12.0891415201762,25.329679981508,9.00624999999999));
#9798=CARTESIAN_POINT('Ctrl Pts',(-11.7670760549233,24.2694595959893,8.725));
#9799=CARTESIAN_POINT('Ctrl Pts',(-10.706938361234,23.946655369415,8.44375));
#9800=CARTESIAN_POINT('Ctrl Pts',(-9.84887002105266,24.6519632977172,8.1625));
#9801=CARTESIAN_POINT('Ctrl Pts',(-9.9417451684382,25.5673438360005,7.92812499999999));
#9802=CARTESIAN_POINT('Ctrl Pts',(-10.446345936791,26.0179944258633,7.740625));
#9803=CARTESIAN_POINT('Ctrl Pts',(-10.772287424497,26.1004782148047,7.646875));
#9804=CARTESIAN_POINT('Ctrl Pts',(-10.9359120418715,26.1004782148047,7.6));
#9805=CARTESIAN_POINT('Ctrl Pts',(-10.9359120418715,26.1004782148047,16.5439001311859));
#9806=CARTESIAN_POINT('Ctrl Pts',(-11.0994822304736,26.1004782148047,16.4970251311859));
#9807=CARTESIAN_POINT('Ctrl Pts',(-11.4254856552641,26.0179777379893,16.4032751311859));
#9808=CARTESIAN_POINT('Ctrl Pts',(-11.9299950149165,25.5673798144889,16.2157751311859));
#9809=CARTESIAN_POINT('Ctrl Pts',(-12.0229600596387,24.6519505470442,15.9814001311859));
#9810=CARTESIAN_POINT('Ctrl Pts',(-11.1648652565317,23.946693336158,15.7001501311859));
#9811=CARTESIAN_POINT('Ctrl Pts',(-10.1047747807049,24.2694732685672,15.4189001311859));
#9812=CARTESIAN_POINT('Ctrl Pts',(-9.78270553499417,25.3296774410397,15.1376501311859));
#9813=CARTESIAN_POINT('Ctrl Pts',(-10.4860435089969,26.1867623778528,14.8564001311859));
#9814=CARTESIAN_POINT('Ctrl Pts',(-11.5890682328979,26.0779917788703,14.5751501311859));
#9815=CARTESIAN_POINT('Ctrl Pts',(-12.1116199022434,25.1004987935522,14.2939001311859));
#9816=CARTESIAN_POINT('Ctrl Pts',(-11.5890871711374,24.1229130219417,14.0126501311859));
#9817=CARTESIAN_POINT('Ctrl Pts',(-10.4859959955657,24.014282423191,13.7314001311859));
#9818=CARTESIAN_POINT('Ctrl Pts',(-9.7828058066508,24.8711088991058,13.4501501311859));
#9819=CARTESIAN_POINT('Ctrl Pts',(-10.1045706423353,25.9318216358326,13.1689001311859));
#9820=CARTESIAN_POINT('Ctrl Pts',(-11.1652784540862,26.2535822819133,12.8876501311859));
#9821=CARTESIAN_POINT('Ctrl Pts',(-12.0221130963663,25.5503976790619,12.6064001311859));
#9822=CARTESIAN_POINT('Ctrl Pts',(-11.9134669344998,24.4472966785626,12.3251501311859));
#9823=CARTESIAN_POINT('Ctrl Pts',(-10.9359120418715,23.9247830105523,12.0439001311859));
#9824=CARTESIAN_POINT('Ctrl Pts',(-9.95835714924316,24.4472966785625,11.7626501311859));
#9825=CARTESIAN_POINT('Ctrl Pts',(-9.84971098737667,25.5503976790619,11.4814001311859));
#9826=CARTESIAN_POINT('Ctrl Pts',(-10.7065456296568,26.2535822819133,11.2001501311859));
#9827=CARTESIAN_POINT('Ctrl Pts',(-11.7672534414077,25.9318216358326,10.9189001311859));
#9828=CARTESIAN_POINT('Ctrl Pts',(-12.0890182770922,24.8711088991058,10.6376501311859));
#9829=CARTESIAN_POINT('Ctrl Pts',(-11.3858280881773,24.014282423191,10.3564001311859));
#9830=CARTESIAN_POINT('Ctrl Pts',(-10.2827369126056,24.1229130219416,10.0751501311859));
#9831=CARTESIAN_POINT('Ctrl Pts',(-9.76020418149962,25.1004987935522,9.7939001311859));
#9832=CARTESIAN_POINT('Ctrl Pts',(-10.2827558508451,26.0779917788702,9.5126501311859));
#9833=CARTESIAN_POINT('Ctrl Pts',(-11.3857805747461,26.1867623778528,9.23140013118589));
#9834=CARTESIAN_POINT('Ctrl Pts',(-12.0891185487488,25.3296774410397,8.9501501311859));
#9835=CARTESIAN_POINT('Ctrl Pts',(-11.7670493030381,24.2694732685672,8.66890013118588));
#9836=CARTESIAN_POINT('Ctrl Pts',(-10.7069588272113,23.946693336158,8.38765013118591));
#9837=CARTESIAN_POINT('Ctrl Pts',(-9.84886402410427,24.6519505470442,8.10640013118589));
#9838=CARTESIAN_POINT('Ctrl Pts',(-9.94182906882648,25.5673798144889,7.8720251311859));
#9839=CARTESIAN_POINT('Ctrl Pts',(-10.4463384284789,26.0179777379893,7.6845251311859));
#9840=CARTESIAN_POINT('Ctrl Pts',(-10.7723418532693,26.1004782148047,7.5907751311859));
#9841=CARTESIAN_POINT('Ctrl Pts',(-10.9359120418715,26.1004782148047,7.5439001311859));
#9842=CARTESIAN_POINT('Ctrl Pts',(-10.9359120418715,26.1266450098064,16.4693527133209));
#9843=CARTESIAN_POINT('Ctrl Pts',(-11.1038344518235,26.1266450098064,16.4224777133209));
#9844=CARTESIAN_POINT('Ctrl Pts',(-11.4382862797329,26.0420078700208,16.3287277133209));
#9845=CARTESIAN_POINT('Ctrl Pts',(-11.9561181415698,25.5795494643233,16.1412277133209));
#9846=CARTESIAN_POINT('Ctrl Pts',(-12.0513966768011,24.640230909128,15.9068527133209));
#9847=CARTESIAN_POINT('Ctrl Pts',(-11.1708833441426,23.9164521808741,15.6256027133209));
#9848=CARTESIAN_POINT('Ctrl Pts',(-10.0829911382721,24.247710417425,15.3443527133209));
#9849=CARTESIAN_POINT('Ctrl Pts',(-9.75249938143592,25.3356782161237,15.0631027133209));
#9850=CARTESIAN_POINT('Ctrl Pts',(-10.4742556343159,26.2152220988022,14.7818527133209));
#9851=CARTESIAN_POINT('Ctrl Pts',(-11.6061804950126,26.1035992577537,14.5006027133209));
#9852=CARTESIAN_POINT('Ctrl Pts',(-12.142419869351,25.1004997827956,14.2193527133209));
#9853=CARTESIAN_POINT('Ctrl Pts',(-11.6061990100998,24.0973030612035,13.9381027133209));
#9854=CARTESIAN_POINT('Ctrl Pts',(-10.4742091825201,23.9858269503648,13.6568527133209));
#9855=CARTESIAN_POINT('Ctrl Pts',(-9.75259741256427,24.8650999474953,13.3756027133209));
#9856=CARTESIAN_POINT('Ctrl Pts',(-10.0827915622055,25.9536007595893,13.0943527133209));
#9857=CARTESIAN_POINT('Ctrl Pts',(-11.1712872924373,26.2837906798065,12.8131027133209));
#9858=CARTESIAN_POINT('Ctrl Pts',(-12.0505688097153,25.5621844389304,12.5318527133209));
#9859=CARTESIAN_POINT('Ctrl Pts',(-11.9390764050646,24.4301849692063,12.2506027133209));
#9860=CARTESIAN_POINT('Ctrl Pts',(-10.9359120418715,23.8939827714609,11.9693527133209));
#9861=CARTESIAN_POINT('Ctrl Pts',(-9.93274767867843,24.4301849692063,11.6881027133209));
#9862=CARTESIAN_POINT('Ctrl Pts',(-9.82125527402764,25.5621844389305,11.4068527133209));
#9863=CARTESIAN_POINT('Ctrl Pts',(-10.7005367913057,26.2837906798064,11.1256027133209));
#9864=CARTESIAN_POINT('Ctrl Pts',(-11.7890325215375,25.9536007595894,10.8443527133209));
#9865=CARTESIAN_POINT('Ctrl Pts',(-12.1192266711787,24.8650999474953,10.5631027133209));
#9866=CARTESIAN_POINT('Ctrl Pts',(-11.3976149012229,23.9858269503648,10.2818527133209));
#9867=CARTESIAN_POINT('Ctrl Pts',(-10.2656250736432,24.0973030612034,10.0006027133209));
#9868=CARTESIAN_POINT('Ctrl Pts',(-9.72940421439204,25.1004997827956,9.7193527133209));
#9869=CARTESIAN_POINT('Ctrl Pts',(-10.2656435887304,26.1035992577537,9.43810271332087));
#9870=CARTESIAN_POINT('Ctrl Pts',(-11.3975684494271,26.2152220988022,9.1568527133209));
#9871=CARTESIAN_POINT('Ctrl Pts',(-12.1193247023071,25.3356782161237,8.87560271332088));
#9872=CARTESIAN_POINT('Ctrl Pts',(-11.7888329454709,24.2477104174249,8.59435271332089));
#9873=CARTESIAN_POINT('Ctrl Pts',(-10.7009407396004,23.9164521808741,8.31310271332088));
#9874=CARTESIAN_POINT('Ctrl Pts',(-9.82042740694183,24.640230909128,8.03185271332089));
#9875=CARTESIAN_POINT('Ctrl Pts',(-9.91570594217325,25.5795494643233,7.79747771332088));
#9876=CARTESIAN_POINT('Ctrl Pts',(-10.4335378040101,26.0420078700208,7.60997771332088));
#9877=CARTESIAN_POINT('Ctrl Pts',(-10.7679896319195,26.1266450098064,7.51622771332088));
#9878=CARTESIAN_POINT('Ctrl Pts',(-10.9359120418715,26.1266450098064,7.46935271332088));
#9879=CARTESIAN_POINT('Ctrl Pts',(-10.9359120418715,26.2066161778899,16.3896589751759));
#9880=CARTESIAN_POINT('Ctrl Pts',(-11.1168911197771,26.2066161778899,16.3427839751759));
#9881=CARTESIAN_POINT('Ctrl Pts',(-11.477441396077,26.1153739493474,16.2490339751759));
#9882=CARTESIAN_POINT('Ctrl Pts',(-12.0355787665632,25.6169041478587,16.0615339751759));
#9883=CARTESIAN_POINT('Ctrl Pts',(-12.1383318463205,24.6043559511596,15.8271589751759));
#9884=CARTESIAN_POINT('Ctrl Pts',(-11.1891838889267,23.8241995587892,15.5459089751759));
#9885=CARTESIAN_POINT('Ctrl Pts',(-10.0165360303049,24.1812600680729,15.2646589751759));
#9886=CARTESIAN_POINT('Ctrl Pts',(-9.66028633666698,25.354006414981,14.9834089751759));
#9887=CARTESIAN_POINT('Ctrl Pts',(-10.4382845848074,26.3020817027312,14.7021589751759));
#9888=CARTESIAN_POINT('Ctrl Pts',(-11.6584070156187,26.1817623874398,14.4209089751759));
#9889=CARTESIAN_POINT('Ctrl Pts',(-12.2364306850993,25.1005012770401,14.1396589751759));
#9890=CARTESIAN_POINT('Ctrl Pts',(-11.6584273539152,24.0191361826963,13.8584089751759));
#9891=CARTESIAN_POINT('Ctrl Pts',(-10.4382335588295,23.8989737631753,13.5771589751759));
#9892=CARTESIAN_POINT('Ctrl Pts',(-9.66039402110579,24.8467593983089,13.2959089751759));
#9893=CARTESIAN_POINT('Ctrl Pts',(-10.0163168012077,26.0200756853628,13.0146589751759));
#9894=CARTESIAN_POINT('Ctrl Pts',(-11.1896276219567,26.3759938775365,12.7334089751759));
#9895=CARTESIAN_POINT('Ctrl Pts',(-12.1374223832382,25.5981603838786,12.4521589751759));
#9896=CARTESIAN_POINT('Ctrl Pts',(-12.0172425339907,24.3779560131358,12.1709089751759));
#9897=CARTESIAN_POINT('Ctrl Pts',(-10.9359120418715,23.7999731705043,11.8896589751759));
#9898=CARTESIAN_POINT('Ctrl Pts',(-9.85458154975225,24.3779560131359,11.6084089751759));
#9899=CARTESIAN_POINT('Ctrl Pts',(-9.73440170050483,25.5981603838786,11.3271589751759));
#9900=CARTESIAN_POINT('Ctrl Pts',(-10.6821964617862,26.3759938775366,11.0459089751759));
#9901=CARTESIAN_POINT('Ctrl Pts',(-11.8555072825353,26.0200756853628,10.7646589751759));
#9902=CARTESIAN_POINT('Ctrl Pts',(-12.2114300626372,24.8467593983089,10.4834089751759));
#9903=CARTESIAN_POINT('Ctrl Pts',(-11.4335905249135,23.8989737631753,10.2021589751759));
#9904=CARTESIAN_POINT('Ctrl Pts',(-10.2133967298278,24.0191361826963,9.92090897517594));
#9905=CARTESIAN_POINT('Ctrl Pts',(-9.63539339864373,25.1005012770401,9.63965897517594));
#9906=CARTESIAN_POINT('Ctrl Pts',(-10.2134170681242,26.1817623874398,9.35840897517593));
#9907=CARTESIAN_POINT('Ctrl Pts',(-11.4335394989356,26.3020817027312,9.07715897517594));
#9908=CARTESIAN_POINT('Ctrl Pts',(-12.211537747076,25.354006414981,8.79590897517593));
#9909=CARTESIAN_POINT('Ctrl Pts',(-11.8552880534381,24.1812600680728,8.51465897517594));
#9910=CARTESIAN_POINT('Ctrl Pts',(-10.6826401948163,23.8241995587893,8.23340897517593));
#9911=CARTESIAN_POINT('Ctrl Pts',(-9.73349223742245,24.6043559511596,7.95215897517595));
#9912=CARTESIAN_POINT('Ctrl Pts',(-9.83624531717977,25.6169041478587,7.71778397517593));
#9913=CARTESIAN_POINT('Ctrl Pts',(-10.394382687666,26.1153739493474,7.53028397517594));
#9914=CARTESIAN_POINT('Ctrl Pts',(-10.7549329639659,26.2066161778899,7.43653397517594));
#9915=CARTESIAN_POINT('Ctrl Pts',(-10.9359120418715,26.2066161778899,7.38965897517594));
#9916=CARTESIAN_POINT('Ctrl Pts',(-10.9359120418715,26.3102987264096,16.3393291535573));
#9917=CARTESIAN_POINT('Ctrl Pts',(-11.1338720637509,26.3102987264096,16.2924541535573));
#9918=CARTESIAN_POINT('Ctrl Pts',(-11.5281986604801,26.2105092515307,16.1987041535573));
#9919=CARTESIAN_POINT('Ctrl Pts',(-12.1386810721185,25.6652994374558,16.0112041535573));
#9920=CARTESIAN_POINT('Ctrl Pts',(-12.2510373785934,24.5578565125378,15.7768291535573));
#9921=CARTESIAN_POINT('Ctrl Pts',(-11.2129304523193,23.7045571560224,15.4955791535573));
#9922=CARTESIAN_POINT('Ctrl Pts',(-9.93035099920634,24.0950939390133,15.2143291535573));
#9923=CARTESIAN_POINT('Ctrl Pts',(-9.54070984355737,25.3777713816557,14.9330791535573));
#9924=CARTESIAN_POINT('Ctrl Pts',(-10.3916362061851,26.414720925681,14.6518291535573));
#9925=CARTESIAN_POINT('Ctrl Pts',(-11.7261342725577,26.283122183649,14.3705791535573));
#9926=CARTESIAN_POINT('Ctrl Pts',(-12.3583416789862,25.1005035455251,14.0893291535573));
#9927=CARTESIAN_POINT('Ctrl Pts',(-11.726156299625,23.9177706952197,13.8080791535573));
#9928=CARTESIAN_POINT('Ctrl Pts',(-10.3915809433155,23.7863442817964,13.5268291535573));
#9929=CARTESIAN_POINT('Ctrl Pts',(-9.54082646945068,24.8229756818914,13.2455791535573));
#9930=CARTESIAN_POINT('Ctrl Pts',(-9.93011356689479,26.1062791264966,12.9643291535573));
#9931=CARTESIAN_POINT('Ctrl Pts',(-11.2134110261814,26.4955612225042,12.6830791535573));
#9932=CARTESIAN_POINT('Ctrl Pts',(-12.2500524410375,25.6448133111173,12.4018291535573));
#9933=CARTESIAN_POINT('Ctrl Pts',(-12.1186068875143,24.3102264920467,12.1205791535573));
#9934=CARTESIAN_POINT('Ctrl Pts',(-10.9359120418715,23.6780633084266,11.8393291535573));
#9935=CARTESIAN_POINT('Ctrl Pts',(-9.75321719622871,24.3102264920467,11.5580791535573));
#9936=CARTESIAN_POINT('Ctrl Pts',(-9.62177164270546,25.6448133111173,11.2768291535573));
#9937=CARTESIAN_POINT('Ctrl Pts',(-10.6584130575616,26.4955612225041,10.9955791535573));
#9938=CARTESIAN_POINT('Ctrl Pts',(-11.9417105168482,26.1062791264966,10.7143291535573));
#9939=CARTESIAN_POINT('Ctrl Pts',(-12.3309976142923,24.8229756818914,10.4330791535573));
#9940=CARTESIAN_POINT('Ctrl Pts',(-11.4802431404275,23.7863442817964,10.1518291535573));
#9941=CARTESIAN_POINT('Ctrl Pts',(-10.1456677841179,23.9177706952197,9.8705791535573));
#9942=CARTESIAN_POINT('Ctrl Pts',(-9.51348240475674,25.100503545525,9.58932915355731));
#9943=CARTESIAN_POINT('Ctrl Pts',(-10.1456898111852,26.283122183649,9.30807915355731));
#9944=CARTESIAN_POINT('Ctrl Pts',(-11.4801878775579,26.414720925681,9.0268291535573));
#9945=CARTESIAN_POINT('Ctrl Pts',(-12.3311142401856,25.3777713816556,8.74557915355731));
#9946=CARTESIAN_POINT('Ctrl Pts',(-11.9414730845367,24.0950939390133,8.4643291535573));
#9947=CARTESIAN_POINT('Ctrl Pts',(-10.6588936314237,23.7045571560224,8.18307915355731));
#9948=CARTESIAN_POINT('Ctrl Pts',(-9.62078670514964,24.5578565125378,7.9018291535573));
#9949=CARTESIAN_POINT('Ctrl Pts',(-9.73314301162452,25.6652994374557,7.66745415355731));
#9950=CARTESIAN_POINT('Ctrl Pts',(-10.3436254232628,26.2105092515307,7.4799541535573));
#9951=CARTESIAN_POINT('Ctrl Pts',(-10.7379520199921,26.3102987264096,7.3862041535573));
#9952=CARTESIAN_POINT('Ctrl Pts',(-10.9359120418715,26.3102987264096,7.3393291535573));
#9953=CARTESIAN_POINT('Ctrl Pts',(-10.9359120418715,26.4672083419587,16.3570635515172));
#9954=CARTESIAN_POINT('Ctrl Pts',(-11.1595402772042,26.4672083419587,16.3101885515172));
#9955=CARTESIAN_POINT('Ctrl Pts',(-11.6050171261006,26.3544745087491,16.2164385515172));
#9956=CARTESIAN_POINT('Ctrl Pts',(-12.2946660690771,25.7385591499254,16.0289385515172));
#9957=CARTESIAN_POINT('Ctrl Pts',(-12.4216053921143,24.4874787891417,15.7945635515172));
#9958=CARTESIAN_POINT('Ctrl Pts',(-11.2488563449896,23.5235154857298,15.5133135515172));
#9959=CARTESIAN_POINT('Ctrl Pts',(-9.79993635312278,23.9647006498918,15.2320635515172));
#9960=CARTESIAN_POINT('Ctrl Pts',(-9.35975960806662,25.4137350597913,14.9508135515172));
#9961=CARTESIAN_POINT('Ctrl Pts',(-10.3210469490048,26.5851705638016,14.6695635515172));
#9962=CARTESIAN_POINT('Ctrl Pts',(-11.8286214898723,26.4365044605197,14.3883135515172));
#9963=CARTESIAN_POINT('Ctrl Pts',(-12.5428227658856,25.100506790018,14.1070635515172));
#9964=CARTESIAN_POINT('Ctrl Pts',(-11.828646456962,23.7643802784334,13.8258135515172));
#9965=CARTESIAN_POINT('Ctrl Pts',(-10.3209843100246,23.6159085765209,13.5445635515172));
#9966=CARTESIAN_POINT('Ctrl Pts',(-9.35989180039454,24.7869851870527,13.2633135515172));
#9967=CARTESIAN_POINT('Ctrl Pts',(-9.79966722986749,26.2367257803968,12.9820635515172));
#9968=CARTESIAN_POINT('Ctrl Pts',(-11.2494010641543,26.676495553443,12.7008135515172));
#9969=CARTESIAN_POINT('Ctrl Pts',(-12.4204889756426,25.715410475817,12.4195635515172));
#9970=CARTESIAN_POINT('Ctrl Pts',(-12.2719956805126,24.2077353396082,12.1383135515172));
#9971=CARTESIAN_POINT('Ctrl Pts',(-10.9359120418715,23.4935841866678,11.8570635515172));
#9972=CARTESIAN_POINT('Ctrl Pts',(-9.59982840323043,24.2077353396082,11.5758135515172));
#9973=CARTESIAN_POINT('Ctrl Pts',(-9.45133510810041,25.715410475817,11.2945635515172));
#9974=CARTESIAN_POINT('Ctrl Pts',(-10.6224230195887,26.676495553443,11.0133135515172));
#9975=CARTESIAN_POINT('Ctrl Pts',(-12.0721568538755,26.2367257803968,10.7320635515172));
#9976=CARTESIAN_POINT('Ctrl Pts',(-12.5119322833484,24.7869851870527,10.4508135515172));
#9977=CARTESIAN_POINT('Ctrl Pts',(-11.5508397737184,23.6159085765208,10.1695635515172));
#9978=CARTESIAN_POINT('Ctrl Pts',(-10.043177626781,23.7643802784334,9.88831355151715));
#9979=CARTESIAN_POINT('Ctrl Pts',(-9.32900131785735,25.100506790018,9.60706355151718));
#9980=CARTESIAN_POINT('Ctrl Pts',(-10.0432025938707,26.4365044605196,9.32581355151715));
#9981=CARTESIAN_POINT('Ctrl Pts',(-11.5507771347382,26.5851705638017,9.04456355151718));
#9982=CARTESIAN_POINT('Ctrl Pts',(-12.5120644756764,25.4137350597913,8.76331355151716));
#9983=CARTESIAN_POINT('Ctrl Pts',(-12.0718877306202,23.9647006498918,8.48206355151717));
#9984=CARTESIAN_POINT('Ctrl Pts',(-10.6229677387534,23.5235154857298,8.20081355151717));
#9985=CARTESIAN_POINT('Ctrl Pts',(-9.45021869162864,24.4874787891416,7.91956355151716));
#9986=CARTESIAN_POINT('Ctrl Pts',(-9.57715801466589,25.7385591499254,7.68518855151717));
#9987=CARTESIAN_POINT('Ctrl Pts',(-10.2668069576424,26.3544745087491,7.49768855151717));
#9988=CARTESIAN_POINT('Ctrl Pts',(-10.7122838065388,26.4672083419587,7.40393855151717));
#9989=CARTESIAN_POINT('Ctrl Pts',(-10.9359120418715,26.4672083419587,7.35706355151717));
#9990=CARTESIAN_POINT('Ctrl Pts',(-10.9359120418715,26.6081512188429,16.4968351856384));
#9991=CARTESIAN_POINT('Ctrl Pts',(-11.1825974273318,26.6081512188429,16.4499601856384));
#9992=CARTESIAN_POINT('Ctrl Pts',(-11.6740186123714,26.4837904806807,16.3562101856384));
#9993=CARTESIAN_POINT('Ctrl Pts',(-12.4347797573637,25.8043635573141,16.1687101856384));
#9994=CARTESIAN_POINT('Ctrl Pts',(-12.5748167258039,24.4242627348399,15.9343351856384));
#9995=CARTESIAN_POINT('Ctrl Pts',(-11.2811268343162,23.3608955651971,15.6530851856383));
#9996=CARTESIAN_POINT('Ctrl Pts',(-9.68279195417932,23.8475756440501,15.3718351856384));
#9997=CARTESIAN_POINT('Ctrl Pts',(-9.1972220581971,25.4460392026774,15.0905851856384));
#9998=CARTESIAN_POINT('Ctrl Pts',(-10.2576404855488,26.7382760883188,14.8093351856384));
#9999=CARTESIAN_POINT('Ctrl Pts',(-11.9206801154866,26.5742792834522,14.5280851856384));
#10000=CARTESIAN_POINT('Ctrl Pts',(-12.7085319370769,25.1005097098055,14.2468351856384));
#10001=CARTESIAN_POINT('Ctrl Pts',(-11.9207077123293,23.6265981302194,13.9655851856384));
#10002=CARTESIAN_POINT('Ctrl Pts',(-10.2575712488811,23.4628155904643,13.6843351856384));
#10003=CARTESIAN_POINT('Ctrl Pts',(-9.19736817418599,24.7546569112497,13.4030851856384));
#10004=CARTESIAN_POINT('Ctrl Pts',(-9.68249448443413,26.3538988103469,13.1218351856384));
#10005=CARTESIAN_POINT('Ctrl Pts',(-11.2817289291307,26.8390188766716,12.8405851856384));
#10006=CARTESIAN_POINT('Ctrl Pts',(-12.5735827078803,25.7788240125713,12.5593351856384));
#10007=CARTESIAN_POINT('Ctrl Pts',(-12.4097763675053,24.1156731939899,12.2780851856384));
#10008=CARTESIAN_POINT('Ctrl Pts',(-10.9359120418715,23.3278767733619,11.9968351856384));
#10009=CARTESIAN_POINT('Ctrl Pts',(-9.46204771623775,24.1156731939899,11.7155851856384));
#10010=CARTESIAN_POINT('Ctrl Pts',(-9.29824137586269,25.7788240125713,11.4343351856384));
#10011=CARTESIAN_POINT('Ctrl Pts',(-10.5900951546124,26.8390188766716,11.1530851856384));
#10012=CARTESIAN_POINT('Ctrl Pts',(-12.1893295993088,26.3538988103469,10.8718351856384));
#10013=CARTESIAN_POINT('Ctrl Pts',(-12.674455909557,24.7546569112497,10.5905851856384));
#10014=CARTESIAN_POINT('Ctrl Pts',(-11.6142528348618,23.4628155904642,10.3093351856384));
#10015=CARTESIAN_POINT('Ctrl Pts',(-9.95111637141368,23.6265981302195,10.0280851856384));
#10016=CARTESIAN_POINT('Ctrl Pts',(-9.16329214666605,25.1005097098054,9.74683518563837));
#10017=CARTESIAN_POINT('Ctrl Pts',(-9.9511439682564,26.5742792834522,9.46558518563839));
#10018=CARTESIAN_POINT('Ctrl Pts',(-11.6141835981942,26.7382760883188,9.18433518563837));
#10019=CARTESIAN_POINT('Ctrl Pts',(-12.6746020255459,25.4460392026774,8.90308518563838));
#10020=CARTESIAN_POINT('Ctrl Pts',(-12.1890321295637,23.8475756440501,8.62183518563838));
#10021=CARTESIAN_POINT('Ctrl Pts',(-10.5906972494268,23.3608955651972,8.34058518563839));
#10022=CARTESIAN_POINT('Ctrl Pts',(-9.29700735793908,24.4242627348399,8.05933518563838));
#10023=CARTESIAN_POINT('Ctrl Pts',(-9.43704432637928,25.8043635573141,7.82496018563839));
#10024=CARTESIAN_POINT('Ctrl Pts',(-10.1978054713715,26.4837904806807,7.63746018563838));
#10025=CARTESIAN_POINT('Ctrl Pts',(-10.6892266564112,26.6081512188429,7.54371018563838));
#10026=CARTESIAN_POINT('Ctrl Pts',(-10.9359120418715,26.6081512188429,7.49683518563838));
#10027=CARTESIAN_POINT('Ctrl Pts',(-10.9359120418715,26.6083071804768,16.7239284079399));
#10028=CARTESIAN_POINT('Ctrl Pts',(-11.1826417158169,26.6083071804768,16.6770534079399));
#10029=CARTESIAN_POINT('Ctrl Pts',(-11.6740923767204,26.4839393326867,16.5833034079399));
#10030=CARTESIAN_POINT('Ctrl Pts',(-12.4349637416248,25.8044239635482,16.3958034079399));
#10031=CARTESIAN_POINT('Ctrl Pts',(-12.5749841946544,24.4241971806872,16.1614284079399));
#10032=CARTESIAN_POINT('Ctrl Pts',(-11.2811696029524,23.3607025205763,15.8801784079399));
#10033=CARTESIAN_POINT('Ctrl Pts',(-9.68265309931028,23.8474413221505,15.5989284079399));
#10034=CARTESIAN_POINT('Ctrl Pts',(-9.19703427713218,25.4460758254194,15.3176784079399));
#10035=CARTESIAN_POINT('Ctrl Pts',(-10.2575660901313,26.7384546586772,15.0364284079399));
#10036=CARTESIAN_POINT('Ctrl Pts',(-11.9207875181861,26.5744393107299,14.7551784079399));
#10037=CARTESIAN_POINT('Ctrl Pts',(-12.7087245360209,25.10050983039,14.4739284079399));
#10038=CARTESIAN_POINT('Ctrl Pts',(-11.9208148787593,23.6264378004142,14.1926784079399));
#10039=CARTESIAN_POINT('Ctrl Pts',(-10.2574974462324,23.4626375379351,13.9114284079399));
#10040=CARTESIAN_POINT('Ctrl Pts',(-9.19717914213288,24.7546192918056,13.6301784079399));
#10041=CARTESIAN_POINT('Ctrl Pts',(-9.68235817663199,26.3540351160508,13.3489284079399));
#10042=CARTESIAN_POINT('Ctrl Pts',(-11.2817665384133,26.8392079241505,13.0676784079399));
#10043=CARTESIAN_POINT('Ctrl Pts',(-12.5737607880012,25.7788977786177,12.7864284079399));
#10044=CARTESIAN_POINT('Ctrl Pts',(-12.4099366382488,24.1155661039636,12.5051784079399));
#10045=CARTESIAN_POINT('Ctrl Pts',(-10.9359120418715,23.3276840193356,12.2239284079399));
#10046=CARTESIAN_POINT('Ctrl Pts',(-9.4618874454942,24.1155661039636,11.9426784079399));
#10047=CARTESIAN_POINT('Ctrl Pts',(-9.29806329574184,25.7788977786177,11.6614284079399));
#10048=CARTESIAN_POINT('Ctrl Pts',(-10.5900575453297,26.8392079241504,11.3801784079399));
#10049=CARTESIAN_POINT('Ctrl Pts',(-12.189465907111,26.3540351160508,11.0989284079399));
#10050=CARTESIAN_POINT('Ctrl Pts',(-12.6746449416101,24.7546192918055,10.8176784079399));
#10051=CARTESIAN_POINT('Ctrl Pts',(-11.6143266375106,23.4626375379351,10.5364284079399));
#10052=CARTESIAN_POINT('Ctrl Pts',(-9.95100920498365,23.6264378004142,10.2551784079399));
#10053=CARTESIAN_POINT('Ctrl Pts',(-9.16309954772204,25.10050983039,9.9739284079399));
#10054=CARTESIAN_POINT('Ctrl Pts',(-9.95103656555694,26.5744393107299,9.6926784079399));
#10055=CARTESIAN_POINT('Ctrl Pts',(-11.6142579936116,26.7384546586772,9.4114284079399));
#10056=CARTESIAN_POINT('Ctrl Pts',(-12.6747898066108,25.4460758254194,9.13017840793991));
#10057=CARTESIAN_POINT('Ctrl Pts',(-12.1891709844327,23.8474413221505,8.84892840793989));
#10058=CARTESIAN_POINT('Ctrl Pts',(-10.5906544807905,23.3607025205763,8.5676784079399));
#10059=CARTESIAN_POINT('Ctrl Pts',(-9.29683988908855,24.4241971806872,8.2864284079399));
#10060=CARTESIAN_POINT('Ctrl Pts',(-9.43686034211822,25.8044239635482,8.05205340793991));
#10061=CARTESIAN_POINT('Ctrl Pts',(-10.1977317070226,26.4839393326867,7.8645534079399));
#10062=CARTESIAN_POINT('Ctrl Pts',(-10.6891823679261,26.6083071804768,7.77080340793991));
#10063=CARTESIAN_POINT('Ctrl Pts',(-10.9359120418715,26.6083071804768,7.7239284079399));
#10064=CARTESIAN_POINT('Ctrl Pts',(-10.9359120418715,26.4141282398751,16.8792407663736));
#10065=CARTESIAN_POINT('Ctrl Pts',(-11.1508380894168,26.4141282398751,16.8323657663736));
#10066=CARTESIAN_POINT('Ctrl Pts',(-11.579033249117,26.3057674496366,16.7386157663736));
#10067=CARTESIAN_POINT('Ctrl Pts',(-12.2418694213241,25.7137890968229,16.5511157663736));
#10068=CARTESIAN_POINT('Ctrl Pts',(-12.3639069611349,24.5112820297777,16.3167407663736));
#10069=CARTESIAN_POINT('Ctrl Pts',(-11.2366960152862,23.5847723620182,16.0354907663736));
#10070=CARTESIAN_POINT('Ctrl Pts',(-9.8440629677261,24.0088154675039,15.7542407663736));
#10071=CARTESIAN_POINT('Ctrl Pts',(-9.4209803113142,25.4015682142421,15.4729907663736));
#10072=CARTESIAN_POINT('Ctrl Pts',(-10.3449304950388,26.5275008077356,15.1917407663736));
#10073=CARTESIAN_POINT('Ctrl Pts',(-11.7939460365568,26.3846099294544,14.9104907663736));
#10074=CARTESIAN_POINT('Ctrl Pts',(-12.4804063041722,25.1005055735222,14.6292407663736));
#10075=CARTESIAN_POINT('Ctrl Pts',(-11.7939702514824,23.8162778614928,14.3479907663736));
#10076=CARTESIAN_POINT('Ctrl Pts',(-10.3448697431333,23.6735731085796,14.0667407663736));
#10077=CARTESIAN_POINT('Ctrl Pts',(-9.42110852120592,24.7991620873381,13.7854907663736));
#10078=CARTESIAN_POINT('Ctrl Pts',(-9.84380195187374,26.192590953643,13.5042407663736));
#10079=CARTESIAN_POINT('Ctrl Pts',(-11.2372243282571,26.6152789310382,13.2229907663736));
#10080=CARTESIAN_POINT('Ctrl Pts',(-12.362824135908,25.6915249005696,12.9417407663736));
#10081=CARTESIAN_POINT('Ctrl Pts',(-12.2200987049739,24.2424118032843,12.6604907663736));
#10082=CARTESIAN_POINT('Ctrl Pts',(-10.9359120418715,23.5560001427465,12.3792407663736));
#10083=CARTESIAN_POINT('Ctrl Pts',(-9.65172537876912,24.2424118032843,12.0979907663736));
#10084=CARTESIAN_POINT('Ctrl Pts',(-9.50899994783496,25.6915249005695,11.8167407663736));
#10085=CARTESIAN_POINT('Ctrl Pts',(-10.6345997554859,26.6152789310382,11.5354907663736));
#10086=CARTESIAN_POINT('Ctrl Pts',(-12.0280221318692,26.192590953643,11.2542407663736));
#10087=CARTESIAN_POINT('Ctrl Pts',(-12.4507155625371,24.7991620873381,10.9729907663736));
#10088=CARTESIAN_POINT('Ctrl Pts',(-11.5269543406097,23.6735731085796,10.6917407663736));
#10089=CARTESIAN_POINT('Ctrl Pts',(-10.0778538322605,23.8162778614928,10.4104907663736));
#10090=CARTESIAN_POINT('Ctrl Pts',(-9.39141777957078,25.1005055735222,10.1292407663736));
#10091=CARTESIAN_POINT('Ctrl Pts',(-10.0778780471862,26.3846099294544,9.84799076637357));
#10092=CARTESIAN_POINT('Ctrl Pts',(-11.5268935887042,26.5275008077356,9.56674076637359));
#10093=CARTESIAN_POINT('Ctrl Pts',(-12.4508437724288,25.4015682142421,9.28549076637358));
#10094=CARTESIAN_POINT('Ctrl Pts',(-12.0277611160169,24.008815467504,9.00424076637358));
#10095=CARTESIAN_POINT('Ctrl Pts',(-10.6351280684568,23.5847723620182,8.72299076637358));
#10096=CARTESIAN_POINT('Ctrl Pts',(-9.5079171226081,24.5112820297778,8.44174076637358));
#10097=CARTESIAN_POINT('Ctrl Pts',(-9.62995466241886,25.7137890968229,8.20736576637358));
#10098=CARTESIAN_POINT('Ctrl Pts',(-10.292790834626,26.3057674496365,8.01986576637358));
#10099=CARTESIAN_POINT('Ctrl Pts',(-10.7209859943261,26.4141282398751,7.92611576637358));
#10100=CARTESIAN_POINT('Ctrl Pts',(-10.9359120418715,26.4141282398751,7.87924076637358));
#10101=CARTESIAN_POINT('Ctrl Pts',(-10.9359120418715,26.1720429125025,16.82358003041));
#10102=CARTESIAN_POINT('Ctrl Pts',(-11.1112963140765,26.1720429125025,16.77670503041));
#10103=CARTESIAN_POINT('Ctrl Pts',(-11.4605069125061,26.0836714981141,16.68295503041));
#10104=CARTESIAN_POINT('Ctrl Pts',(-12.0013030996622,25.6007219425128,16.49545503041));
#10105=CARTESIAN_POINT('Ctrl Pts',(-12.1007423973834,24.6198771550135,16.26108003041));
#10106=CARTESIAN_POINT('Ctrl Pts',(-11.1812909210561,23.8640475726204,15.97983003041));
#10107=CARTESIAN_POINT('Ctrl Pts',(-10.0452414973032,24.2099754626599,15.69858003041));
#10108=CARTESIAN_POINT('Ctrl Pts',(-9.70013098088765,25.3460850661404,15.41733003041));
#10109=CARTESIAN_POINT('Ctrl Pts',(-10.4538244039853,26.2645547246601,15.13608003041));
#10110=CARTESIAN_POINT('Ctrl Pts',(-11.635843063436,26.14799088929,14.85483003041));
#10111=CARTESIAN_POINT('Ctrl Pts',(-12.1958123010896,25.1005009427962,14.57358003041));
#10112=CARTESIAN_POINT('Ctrl Pts',(-11.6358619781388,24.0529085194103,14.29233003041));
#10113=CARTESIAN_POINT('Ctrl Pts',(-10.4537769496115,23.9364993059084,14.01108003041));
#10114=CARTESIAN_POINT('Ctrl Pts',(-9.70023112780759,24.854683509662,13.72983003041));
#10115=CARTESIAN_POINT('Ctrl Pts',(-10.0450376142545,25.9913547946694,13.44858003041));
#10116=CARTESIAN_POINT('Ctrl Pts',(-11.1817035797842,26.3361568964569,13.16733003041));
#10117=CARTESIAN_POINT('Ctrl Pts',(-12.0998967445887,25.5826167555775,12.88608003041));
#10118=CARTESIAN_POINT('Ctrl Pts',(-11.9834703687346,24.4005218591871,12.60483003041));
#10119=CARTESIAN_POINT('Ctrl Pts',(-10.9359120418715,23.8405906121891,12.32358003041));
#10120=CARTESIAN_POINT('Ctrl Pts',(-9.88835371500838,24.4005218591871,12.04233003041));
#10121=CARTESIAN_POINT('Ctrl Pts',(-9.77192733915425,25.5826167555775,11.76108003041));
#10122=CARTESIAN_POINT('Ctrl Pts',(-10.6901205039588,26.3361568964569,11.47983003041));
#10123=CARTESIAN_POINT('Ctrl Pts',(-11.8267864694885,25.9913547946694,11.19858003041));
#10124=CARTESIAN_POINT('Ctrl Pts',(-12.1715929559354,24.854683509662,10.91733003041));
#10125=CARTESIAN_POINT('Ctrl Pts',(-11.4180471341314,23.9364993059084,10.63608003041));
#10126=CARTESIAN_POINT('Ctrl Pts',(-10.2359621056042,24.0529085194103,10.35483003041));
#10127=CARTESIAN_POINT('Ctrl Pts',(-9.6760117826534,25.1005009427962,10.07358003041));
#10128=CARTESIAN_POINT('Ctrl Pts',(-10.2359810203069,26.14799088929,9.79233003040999));
#10129=CARTESIAN_POINT('Ctrl Pts',(-11.4179996797577,26.2645547246602,9.51108003040999));
#10130=CARTESIAN_POINT('Ctrl Pts',(-12.1716931028553,25.3460850661404,9.22983003040999));
#10131=CARTESIAN_POINT('Ctrl Pts',(-11.8265825864398,24.2099754626599,8.94858003040999));
#10132=CARTESIAN_POINT('Ctrl Pts',(-10.6905331626869,23.8640475726204,8.66733003040999));
#10133=CARTESIAN_POINT('Ctrl Pts',(-9.77108168635966,24.6198771550135,8.38608003040999));
#10134=CARTESIAN_POINT('Ctrl Pts',(-9.8705209840808,25.6007219425128,8.15170503040999));
#10135=CARTESIAN_POINT('Ctrl Pts',(-10.4113171712369,26.0836714981141,7.96420503040999));
#10136=CARTESIAN_POINT('Ctrl Pts',(-10.7605277696664,26.1720429125025,7.87045503040999));
#10137=CARTESIAN_POINT('Ctrl Pts',(-10.9359120418715,26.1720429125025,7.82358003040999));
#10138=CARTESIAN_POINT('Ctrl Pts',(-10.9359120418715,26.1004782148047,16.6747998250855));
#10139=CARTESIAN_POINT('Ctrl Pts',(-11.0994166034008,26.1004782148047,16.6279248250855));
#10140=CARTESIAN_POINT('Ctrl Pts',(-11.4254947083535,26.0179576167138,16.5341748250855));
#10141=CARTESIAN_POINT('Ctrl Pts',(-11.9298938526699,25.5674231952741,16.3466748250855));
#10142=CARTESIAN_POINT('Ctrl Pts',(-12.022967290413,24.6519351730184,16.1122998250855));
#10143=CARTESIAN_POINT('Ctrl Pts',(-11.1648405798372,23.9467391142659,15.8310498250855));
#10144=CARTESIAN_POINT('Ctrl Pts',(-10.1048070365844,24.2694897541725,15.5497998250855));
#10145=CARTESIAN_POINT('Ctrl Pts',(-9.78273323261569,25.3296743778897,15.2685498250855));
#10146=CARTESIAN_POINT('Ctrl Pts',(-10.4860583036714,26.1867303933138,14.9872998250855));
#10147=CARTESIAN_POINT('Ctrl Pts',(-11.5890488871064,26.0779653129614,14.7060498250855));
#10148=CARTESIAN_POINT('Ctrl Pts',(-12.111587631401,25.100498383335,14.4247998250855));
#10149=CARTESIAN_POINT('Ctrl Pts',(-11.5890686614131,24.1229405170205,14.1435498250855));
#10150=CARTESIAN_POINT('Ctrl Pts',(-10.486008692659,24.0143126461238,13.8622998250855));
#10151=CARTESIAN_POINT('Ctrl Pts',(-9.7828379310398,24.8711153529452,13.5810498250855));
#10152=CARTESIAN_POINT('Ctrl Pts',(-10.1045938851323,25.9317984014709,13.2997998250855));
#10153=CARTESIAN_POINT('Ctrl Pts',(-11.1652720341777,26.2535501024307,13.0185498250855));
#10154=CARTESIAN_POINT('Ctrl Pts',(-12.0220827798711,25.5503851117544,12.7372998250855));
#10155=CARTESIAN_POINT('Ctrl Pts',(-11.9134396402228,24.4473149177691,12.4560498250855));
#10156=CARTESIAN_POINT('Ctrl Pts',(-10.9359120418715,23.9248158302944,12.1747998250855));
#10157=CARTESIAN_POINT('Ctrl Pts',(-9.95838444352014,24.4473149177691,11.8935498250855));
#10158=CARTESIAN_POINT('Ctrl Pts',(-9.84974130387186,25.5503851117544,11.6122998250855));
#10159=CARTESIAN_POINT('Ctrl Pts',(-10.7065520495652,26.2535501024307,11.3310498250855));
#10160=CARTESIAN_POINT('Ctrl Pts',(-11.7672301986107,25.9317984014709,11.0497998250855));
#10161=CARTESIAN_POINT('Ctrl Pts',(-12.0889861527032,24.8711153529452,10.7685498250855));
#10162=CARTESIAN_POINT('Ctrl Pts',(-11.385815391084,24.0143126461239,10.4872998250855));
#10163=CARTESIAN_POINT('Ctrl Pts',(-10.2827554223299,24.1229405170204,10.2060498250855));
#10164=CARTESIAN_POINT('Ctrl Pts',(-9.76023645234196,25.100498383335,9.92479982508547));
#10165=CARTESIAN_POINT('Ctrl Pts',(-10.2827751966365,26.0779653129613,9.64354982508548));
#10166=CARTESIAN_POINT('Ctrl Pts',(-11.3857657800716,26.1867303933138,9.36229982508546));
#10167=CARTESIAN_POINT('Ctrl Pts',(-12.0890908511273,25.3296743778897,9.08104982508548));
#10168=CARTESIAN_POINT('Ctrl Pts',(-11.7670170471586,24.2694897541725,8.79979982508546));
#10169=CARTESIAN_POINT('Ctrl Pts',(-10.7069835039058,23.9467391142658,8.51854982508547));
#10170=CARTESIAN_POINT('Ctrl Pts',(-9.84885679332996,24.6519351730184,8.23729982508548));
#10171=CARTESIAN_POINT('Ctrl Pts',(-9.94193023107313,25.5674231952741,8.00292482508547));
#10172=CARTESIAN_POINT('Ctrl Pts',(-10.4463293753895,26.0179576167137,7.81542482508547));
#10173=CARTESIAN_POINT('Ctrl Pts',(-10.7724074803422,26.1004782148047,7.72167482508547));
#10174=CARTESIAN_POINT('Ctrl Pts',(-10.9359120418715,26.1004782148047,7.67479982508547));
#10175=CARTESIAN_POINT('Ctrl Pts',(-10.9359120418715,26.1004782148047,16.6));
#10176=CARTESIAN_POINT('Ctrl Pts',(-11.099536659246,26.1004782148047,16.553125));
#10177=CARTESIAN_POINT('Ctrl Pts',(-11.425478146952,26.0179944258633,16.459375));
#10178=CARTESIAN_POINT('Ctrl Pts',(-11.9300789153048,25.5673438360005,16.271875));
#10179=CARTESIAN_POINT('Ctrl Pts',(-12.0229540626903,24.6519632977172,16.0375));
#10180=CARTESIAN_POINT('Ctrl Pts',(-11.164885722509,23.9466553694149,15.75625));
#10181=CARTESIAN_POINT('Ctrl Pts',(-10.1047480288197,24.2694595959893,15.475));
#10182=CARTESIAN_POINT('Ctrl Pts',(-9.7826825635668,25.329679981508,15.19375));
#10183=CARTESIAN_POINT('Ctrl Pts',(-10.4860312388173,26.1867889046978,14.9125));
#10184=CARTESIAN_POINT('Ctrl Pts',(-11.5890842776128,26.0780137287588,14.63125));
#10185=CARTESIAN_POINT('Ctrl Pts',(-12.1116466665383,25.1004991337717,14.35));
#10186=CARTESIAN_POINT('Ctrl Pts',(-11.5891025224479,24.1228902184961,14.06875));
#10187=CARTESIAN_POINT('Ctrl Pts',(-10.4859854650458,24.0142573573597,13.7875));
#10188=CARTESIAN_POINT('Ctrl Pts',(-9.78277916381912,24.8711035465199,13.50625));
#10189=CARTESIAN_POINT('Ctrl Pts',(-10.1045513655818,25.9318409055902,13.225));
#10190=CARTESIAN_POINT('Ctrl Pts',(-11.1652837785312,26.2536089704377,12.94375));
#10191=CARTESIAN_POINT('Ctrl Pts',(-12.0221382397948,25.5504081019422,12.6625));
#10192=CARTESIAN_POINT('Ctrl Pts',(-11.9134895714075,24.4472815516099,12.38125));
#10193=CARTESIAN_POINT('Ctrl Pts',(-10.9359120418715,23.9247557910194,12.1));
#10194=CARTESIAN_POINT('Ctrl Pts',(-9.95833451233548,24.4472815516099,11.81875));
#10195=CARTESIAN_POINT('Ctrl Pts',(-9.84968584394817,25.5504081019422,11.5375));
#10196=CARTESIAN_POINT('Ctrl Pts',(-10.7065403052118,26.2536089704376,11.25625));
#10197=CARTESIAN_POINT('Ctrl Pts',(-11.7672727181612,25.9318409055902,10.975));
#10198=CARTESIAN_POINT('Ctrl Pts',(-12.0890449199239,24.8711035465198,10.69375));
#10199=CARTESIAN_POINT('Ctrl Pts',(-11.3858386186972,24.0142573573597,10.4125));
#10200=CARTESIAN_POINT('Ctrl Pts',(-10.2827215612951,24.1228902184961,10.13125));
#10201=CARTESIAN_POINT('Ctrl Pts',(-9.76017741720471,25.1004991337717,9.85000000000001));
#10202=CARTESIAN_POINT('Ctrl Pts',(-10.2827398061301,26.0780137287587,9.56874999999999));
#10203=CARTESIAN_POINT('Ctrl Pts',(-11.3857928449257,26.1867889046978,9.28750000000001));
#10204=CARTESIAN_POINT('Ctrl Pts',(-12.0891415201762,25.329679981508,9.00624999999999));
#10205=CARTESIAN_POINT('Ctrl Pts',(-11.7670760549233,24.2694595959893,8.725));
#10206=CARTESIAN_POINT('Ctrl Pts',(-10.706938361234,23.946655369415,8.44375));
#10207=CARTESIAN_POINT('Ctrl Pts',(-9.84887002105266,24.6519632977172,8.1625));
#10208=CARTESIAN_POINT('Ctrl Pts',(-9.9417451684382,25.5673438360005,7.92812499999999));
#10209=CARTESIAN_POINT('Ctrl Pts',(-10.446345936791,26.0179944258633,7.740625));
#10210=CARTESIAN_POINT('Ctrl Pts',(-10.772287424497,26.1004782148047,7.646875));
#10211=CARTESIAN_POINT('Ctrl Pts',(-10.9359120418715,26.1004782148047,7.6));
#10212=CARTESIAN_POINT('',(-10.9359120418715,26.1004782148047,7.6));
#10213=CARTESIAN_POINT('Ctrl Pts',(-10.9359120418715,26.1004782148047,16.6));
#10214=CARTESIAN_POINT('Ctrl Pts',(-11.099536659246,26.1004782148047,16.553125));
#10215=CARTESIAN_POINT('Ctrl Pts',(-11.425478146952,26.0179944258633,16.459375));
#10216=CARTESIAN_POINT('Ctrl Pts',(-11.9300789153048,25.5673438360005,16.271875));
#10217=CARTESIAN_POINT('Ctrl Pts',(-12.0229540626903,24.6519632977172,16.0375));
#10218=CARTESIAN_POINT('Ctrl Pts',(-11.164885722509,23.9466553694149,15.75625));
#10219=CARTESIAN_POINT('Ctrl Pts',(-10.1047480288197,24.2694595959893,15.475));
#10220=CARTESIAN_POINT('Ctrl Pts',(-9.7826825635668,25.329679981508,15.19375));
#10221=CARTESIAN_POINT('Ctrl Pts',(-10.4860312388173,26.1867889046978,14.9125));
#10222=CARTESIAN_POINT('Ctrl Pts',(-11.5890842776128,26.0780137287588,14.63125));
#10223=CARTESIAN_POINT('Ctrl Pts',(-12.1116466665383,25.1004991337717,14.35));
#10224=CARTESIAN_POINT('Ctrl Pts',(-11.5891025224479,24.1228902184961,14.06875));
#10225=CARTESIAN_POINT('Ctrl Pts',(-10.4859854650458,24.0142573573597,13.7875));
#10226=CARTESIAN_POINT('Ctrl Pts',(-9.78277916381912,24.8711035465199,13.50625));
#10227=CARTESIAN_POINT('Ctrl Pts',(-10.1045513655818,25.9318409055902,13.225));
#10228=CARTESIAN_POINT('Ctrl Pts',(-11.1652837785312,26.2536089704377,12.94375));
#10229=CARTESIAN_POINT('Ctrl Pts',(-12.0221382397948,25.5504081019422,12.6625));
#10230=CARTESIAN_POINT('Ctrl Pts',(-11.9134895714075,24.4472815516099,12.38125));
#10231=CARTESIAN_POINT('Ctrl Pts',(-10.9359120418715,23.9247557910194,12.1));
#10232=CARTESIAN_POINT('Ctrl Pts',(-9.95833451233548,24.4472815516099,11.81875));
#10233=CARTESIAN_POINT('Ctrl Pts',(-9.84968584394817,25.5504081019422,11.5375));
#10234=CARTESIAN_POINT('Ctrl Pts',(-10.7065403052118,26.2536089704376,11.25625));
#10235=CARTESIAN_POINT('Ctrl Pts',(-11.7672727181612,25.9318409055902,10.975));
#10236=CARTESIAN_POINT('Ctrl Pts',(-12.0890449199239,24.8711035465198,10.69375));
#10237=CARTESIAN_POINT('Ctrl Pts',(-11.3858386186972,24.0142573573597,10.4125));
#10238=CARTESIAN_POINT('Ctrl Pts',(-10.2827215612951,24.1228902184961,10.13125));
#10239=CARTESIAN_POINT('Ctrl Pts',(-9.76017741720471,25.1004991337717,9.85000000000001));
#10240=CARTESIAN_POINT('Ctrl Pts',(-10.2827398061301,26.0780137287587,9.56874999999999));
#10241=CARTESIAN_POINT('Ctrl Pts',(-11.3857928449257,26.1867889046978,9.28750000000001));
#10242=CARTESIAN_POINT('Ctrl Pts',(-12.0891415201762,25.329679981508,9.00624999999999));
#10243=CARTESIAN_POINT('Ctrl Pts',(-11.7670760549233,24.2694595959893,8.725));
#10244=CARTESIAN_POINT('Ctrl Pts',(-10.706938361234,23.946655369415,8.44375));
#10245=CARTESIAN_POINT('Ctrl Pts',(-9.84887002105266,24.6519632977172,8.1625));
#10246=CARTESIAN_POINT('Ctrl Pts',(-9.9417451684382,25.5673438360005,7.92812499999999));
#10247=CARTESIAN_POINT('Ctrl Pts',(-10.446345936791,26.0179944258633,7.740625));
#10248=CARTESIAN_POINT('Ctrl Pts',(-10.772287424497,26.1004782148047,7.646875));
#10249=CARTESIAN_POINT('Ctrl Pts',(-10.9359120418715,26.1004782148047,7.6));
#10250=CARTESIAN_POINT('Origin',(-10.9359120418715,26.3504782148047,7.6));
#10251=CARTESIAN_POINT('Origin',(-10.9359120418715,26.3504782148047,7.6));
#10252=CARTESIAN_POINT('',(0.,0.,0.));
#10253=CARTESIAN_POINT('Origin',(-3.64952178519528,19.0640879581285,17.6));
#10254=CARTESIAN_POINT('',(-3.64952178519528,19.0640879581285,18.35));
#10255=CARTESIAN_POINT('Origin',(-3.64952178519528,19.0640879581285,18.6));
#10256=CARTESIAN_POINT('Origin',(-3.64952178519528,19.0640879581285,17.6));
#10257=CARTESIAN_POINT('',(-3.39952178519528,19.0640879581285,16.6));
#10258=CARTESIAN_POINT('',(-3.89952178519528,19.0640879581285,16.6));
#10259=CARTESIAN_POINT('Origin',(-3.64952178519528,19.0640879581285,16.6));
#10260=CARTESIAN_POINT('Ctrl Pts',(-3.39952178519528,19.0640879581285,16.6));
#10261=CARTESIAN_POINT('Ctrl Pts',(-3.39952178519528,19.0597806646461,16.5977092724426));
#10262=CARTESIAN_POINT('Ctrl Pts',(-3.39955324129755,19.0554410535254,16.5954788663774));
#10263=CARTESIAN_POINT('Ctrl Pts',(-3.40014364770956,19.0127459875283,16.5742560748851));
#10264=CARTESIAN_POINT('Ctrl Pts',(-3.40282286847409,18.9716935753448,16.559542959919));
#10265=CARTESIAN_POINT('Ctrl Pts',(-3.40690999909243,18.9298891387388,16.5481972195909));
#10266=CARTESIAN_POINT('Ctrl Pts',(-3.40698112962582,18.9291660315159,16.5480020646239));
#10267=CARTESIAN_POINT('Ctrl Pts',(-3.4081629902897,18.9172240770089,16.544797109728));
#10268=CARTESIAN_POINT('Ctrl Pts',(-3.409384175847,18.905936706496,16.5420298581508));
#10269=CARTESIAN_POINT('Ctrl Pts',(-3.41126371924574,18.889929722745,16.5384418503857));
#10270=CARTESIAN_POINT('Ctrl Pts',(-3.4118338437146,18.8852272650427,16.5374286265409));
#10271=CARTESIAN_POINT('Ctrl Pts',(-3.41287366194149,18.8769152925628,16.5357072275207));
#10272=CARTESIAN_POINT('Ctrl Pts',(-3.41333572893562,18.8733067646504,16.5349829852478));
#10273=CARTESIAN_POINT('Ctrl Pts',(-3.41433854491902,18.8656535215358,16.5334946079531));
#10274=CARTESIAN_POINT('Ctrl Pts',(-3.41488223353522,18.8616071709856,16.5327358435474));
#10275=CARTESIAN_POINT('Ctrl Pts',(-3.4162295106395,18.8518266202365,16.5309679692519));
#10276=CARTESIAN_POINT('Ctrl Pts',(-3.41704752686023,18.8460875459453,16.5299854641958));
#10277=CARTESIAN_POINT('Ctrl Pts',(-3.4199708406405,18.8262612081367,16.5267739133408));
#10278=CARTESIAN_POINT('Ctrl Pts',(-3.42222357481902,18.8121330333764,16.5248034466825));
#10279=CARTESIAN_POINT('Ctrl Pts',(-3.43123014519201,18.7599127812053,16.5186110231589));
#10280=CARTESIAN_POINT('Ctrl Pts',(-3.4391986219584,18.7214946617958,16.5162061142361));
#10281=CARTESIAN_POINT('Ctrl Pts',(-3.45515688387283,18.6586436195296,16.5154725363415));
#10282=CARTESIAN_POINT('Ctrl Pts',(-3.46228620261987,18.6336658536588,16.5160451884648));
#10283=CARTESIAN_POINT('Ctrl Pts',(-3.49512947595985,18.5324932763169,16.5219235534991));
#10284=CARTESIAN_POINT('Ctrl Pts',(-3.52630916660788,18.4660472824376,16.5341985199053));
#10285=CARTESIAN_POINT('Ctrl Pts',(-3.59133594943102,18.3724026680879,16.5639151059098));
#10286=CARTESIAN_POINT('Ctrl Pts',(-3.62203715988421,18.3415254901727,16.5791986989673));
#10287=CARTESIAN_POINT('Ctrl Pts',(-3.67499828617909,18.306956937443,16.605627659773));
#10288=CARTESIAN_POINT('Ctrl Pts',(-3.69704039179924,18.2980988346278,16.6166575639151));
#10289=CARTESIAN_POINT('Ctrl Pts',(-3.73479375210779,18.2922551407825,16.6350648852536));
#10290=CARTESIAN_POINT('Ctrl Pts',(-3.75139876442454,18.2929258201185,16.6429988757827));
#10291=CARTESIAN_POINT('Ctrl Pts',(-3.78199607956949,18.301731549649,16.6569651923278));
#10292=CARTESIAN_POINT('Ctrl Pts',(-3.79535203986082,18.3088054563803,16.6627780404676));
#10293=CARTESIAN_POINT('Ctrl Pts',(-3.82105390005994,18.3293269577824,16.6732083185761));
#10294=CARTESIAN_POINT('Ctrl Pts',(-3.83248647058025,18.3428683869631,16.677362768157));
#10295=CARTESIAN_POINT('Ctrl Pts',(-3.85612750484055,18.3800246546226,16.6848437491615));
#10296=CARTESIAN_POINT('Ctrl Pts',(-3.86624809413459,18.4053078595428,16.686910649375));
#10297=CARTESIAN_POINT('Ctrl Pts',(-3.88756792802042,18.4782927145015,16.6888104810606));
#10298=CARTESIAN_POINT('Ctrl Pts',(-3.89396521465656,18.5328116182588,16.6853604690573));
#10299=CARTESIAN_POINT('Ctrl Pts',(-3.90307097190431,18.7018817770723,16.6690502405298));
#10300=CARTESIAN_POINT('Ctrl Pts',(-3.89916166722153,18.9142796138527,16.6427595546923));
#10301=CARTESIAN_POINT('Ctrl Pts',(-3.89951831852135,19.058896367419,16.6015112866721));
#10302=CARTESIAN_POINT('Ctrl Pts',(-3.89952178519528,19.0614934249741,16.6007604391535));
#10303=CARTESIAN_POINT('Ctrl Pts',(-3.89952178519528,19.0640879581285,16.6));
#10304=CARTESIAN_POINT('Ctrl Pts',(-3.89952178519528,19.0640879581285,16.6));
#10305=CARTESIAN_POINT('Ctrl Pts',(-3.89952178519528,18.900463340754,16.553125));
#10306=CARTESIAN_POINT('Ctrl Pts',(-3.98201667654796,18.574558453354,16.459375));
#10307=CARTESIAN_POINT('Ctrl Pts',(-4.43261252959751,18.0698369774179,16.271875));
#10308=CARTESIAN_POINT('Ctrl Pts',(-5.3480450944344,17.9770695761824,16.0375));
#10309=CARTESIAN_POINT('Ctrl Pts',(-6.05333812005169,18.8351088887249,15.75625));
#10310=CARTESIAN_POINT('Ctrl Pts',(-5.73053324403457,19.8952490922453,15.475));
#10311=CARTESIAN_POINT('Ctrl Pts',(-4.67032445705031,20.2173120687642,15.19375));
#10312=CARTESIAN_POINT('Ctrl Pts',(-3.81321396620606,19.5139658030124,14.9125));
#10313=CARTESIAN_POINT('Ctrl Pts',(-3.92199288032869,18.4109195983283,14.63125));
#10314=CARTESIAN_POINT('Ctrl Pts',(-4.89949977532975,17.8883587658141,14.35));
#10315=CARTESIAN_POINT('Ctrl Pts',(-5.87710555996492,18.4109010214894,14.06875));
#10316=CARTESIAN_POINT('Ctrl Pts',(-5.98573683407846,19.5140121151019,13.7875));
#10317=CARTESIAN_POINT('Ctrl Pts',(-5.1288955300064,20.2172151824403,13.50625));
#10318=CARTESIAN_POINT('Ctrl Pts',(-4.06816311909486,19.8954444250534,13.225));
#10319=CARTESIAN_POINT('Ctrl Pts',(-3.74639685722716,18.8347173994404,12.94375));
#10320=CARTESIAN_POINT('Ctrl Pts',(-4.44959410269395,17.9778671655289,12.6625));
#10321=CARTESIAN_POINT('Ctrl Pts',(-5.55271521450753,18.0865153161182,12.38125));
#10322=CARTESIAN_POINT('Ctrl Pts',(-6.07523831702883,19.0640879581285,12.1));
#10323=CARTESIAN_POINT('Ctrl Pts',(-5.55271521450754,20.0416606001388,11.81875));
#10324=CARTESIAN_POINT('Ctrl Pts',(-4.44959410269395,20.1503087507281,11.5375));
#10325=CARTESIAN_POINT('Ctrl Pts',(-3.74639685722716,19.2934585168167,11.25625));
#10326=CARTESIAN_POINT('Ctrl Pts',(-4.06816311909486,18.2327314912035,10.975));
#10327=CARTESIAN_POINT('Ctrl Pts',(-5.12889553000641,17.9109607338168,10.69375));
#10328=CARTESIAN_POINT('Ctrl Pts',(-5.98573683407846,18.6141638011551,10.4125));
#10329=CARTESIAN_POINT('Ctrl Pts',(-5.87710555996491,19.7172748947676,10.13125));
#10330=CARTESIAN_POINT('Ctrl Pts',(-4.89949977532976,20.2398171504429,9.84999999999999));
#10331=CARTESIAN_POINT('Ctrl Pts',(-3.92199288032869,19.7172563179287,9.56875000000001));
#10332=CARTESIAN_POINT('Ctrl Pts',(-3.81321396620606,18.6142101132445,9.2875));
#10333=CARTESIAN_POINT('Ctrl Pts',(-4.67032445705031,17.9108638474928,9.00625));
#10334=CARTESIAN_POINT('Ctrl Pts',(-5.73053324403456,18.2329268240116,8.725));
#10335=CARTESIAN_POINT('Ctrl Pts',(-6.05333812005169,19.2930670275321,8.44375));
#10336=CARTESIAN_POINT('Ctrl Pts',(-5.34804509443441,20.1511063400746,8.1625));
#10337=CARTESIAN_POINT('Ctrl Pts',(-4.43261252959751,20.0583389388391,7.928125));
#10338=CARTESIAN_POINT('Ctrl Pts',(-3.98201667654797,19.553617462903,7.740625));
#10339=CARTESIAN_POINT('Ctrl Pts',(-3.89952178519528,19.227712575503,7.646875));
#10340=CARTESIAN_POINT('Ctrl Pts',(-3.89952178519528,19.0640879581285,7.6));
#10341=CARTESIAN_POINT('Ctrl Pts',(-3.89952178519528,19.0640879581285,16.5439001311859));
#10342=CARTESIAN_POINT('Ctrl Pts',(-3.89952178519528,18.9005177695264,16.4970251311859));
#10343=CARTESIAN_POINT('Ctrl Pts',(-3.98203155066432,18.5745451572477,16.4032751311859));
#10344=CARTESIAN_POINT('Ctrl Pts',(-4.43258128086462,18.069910268813,16.2157751311859));
#10345=CARTESIAN_POINT('Ctrl Pts',(-5.34805771398083,17.9770594719705,15.9814001311859));
#10346=CARTESIAN_POINT('Ctrl Pts',(-6.05330733378122,18.8351274602905,15.7001501311859));
#10347=CARTESIAN_POINT('Ctrl Pts',(-5.73052337118203,19.8952269466501,15.4189001311859));
#10348=CARTESIAN_POINT('Ctrl Pts',(-4.67032604039948,20.2172950047912,15.1376501311859));
#10349=CARTESIAN_POINT('Ctrl Pts',(-3.81323472979947,19.5139559069796,14.8564001311859));
#10350=CARTESIAN_POINT('Ctrl Pts',(-3.92200978317002,18.4109322349158,14.5751501311859));
#10351=CARTESIAN_POINT('Ctrl Pts',(-4.89950009636116,17.8883794033646,14.2939001311859));
#10352=CARTESIAN_POINT('Ctrl Pts',(-5.87708785680175,18.4109129736201,14.0126501311859));
#10353=CARTESIAN_POINT('Ctrl Pts',(-5.98571742362024,19.5140039254276,13.7314001311859));
#10354=CARTESIAN_POINT('Ctrl Pts',(-5.12889137335883,20.2171945486251,13.4501501311859));
#10355=CARTESIAN_POINT('Ctrl Pts',(-4.06817805776782,19.8954294777376,13.1689001311859));
#10356=CARTESIAN_POINT('Ctrl Pts',(-3.74641753885177,18.8347215298249,12.8876501311859));
#10357=CARTESIAN_POINT('Ctrl Pts',(-4.44960218182391,17.9778866501029,12.6064001311859));
#10358=CARTESIAN_POINT('Ctrl Pts',(-5.55270349015047,18.0865328607765,12.3251501311859));
#10359=CARTESIAN_POINT('Ctrl Pts',(-6.07521722219095,19.0640879581285,12.0439001311859));
#10360=CARTESIAN_POINT('Ctrl Pts',(-5.55270349015046,20.0416430554805,11.7626501311859));
#10361=CARTESIAN_POINT('Ctrl Pts',(-4.44960218182392,20.1502892661541,11.4814001311859));
#10362=CARTESIAN_POINT('Ctrl Pts',(-3.74641753885177,19.2934543864321,11.2001501311859));
#10363=CARTESIAN_POINT('Ctrl Pts',(-4.06817805776782,18.2327464385194,10.9189001311859));
#10364=CARTESIAN_POINT('Ctrl Pts',(-5.12889137335884,17.910981367632,10.6376501311859));
#10365=CARTESIAN_POINT('Ctrl Pts',(-5.98571742362024,18.6141719908294,10.3564001311859));
#10366=CARTESIAN_POINT('Ctrl Pts',(-5.87708785680175,19.7172629426369,10.0751501311859));
#10367=CARTESIAN_POINT('Ctrl Pts',(-4.89950009636117,20.2397965128924,9.79390013118589));
#10368=CARTESIAN_POINT('Ctrl Pts',(-3.92200978317001,19.7172436813412,9.5126501311859));
#10369=CARTESIAN_POINT('Ctrl Pts',(-3.81323472979948,18.6142200092774,9.23140013118589));
#10370=CARTESIAN_POINT('Ctrl Pts',(-4.67032604039947,17.9108809114658,8.9501501311859));
#10371=CARTESIAN_POINT('Ctrl Pts',(-5.73052337118204,18.2329489696068,8.6689001311859));
#10372=CARTESIAN_POINT('Ctrl Pts',(-6.05330733378122,19.2930484559666,8.38765013118589));
#10373=CARTESIAN_POINT('Ctrl Pts',(-5.34805771398083,20.1511164442865,8.1064001311859));
#10374=CARTESIAN_POINT('Ctrl Pts',(-4.43258128086462,20.058265647444,7.87202513118589));
#10375=CARTESIAN_POINT('Ctrl Pts',(-3.98203155066433,19.5536307590093,7.6845251311859));
#10376=CARTESIAN_POINT('Ctrl Pts',(-3.89952178519528,19.2276581467307,7.5907751311859));
#10377=CARTESIAN_POINT('Ctrl Pts',(-3.89952178519528,19.0640879581285,7.5439001311859));
#10378=CARTESIAN_POINT('Ctrl Pts',(-3.87336343711624,19.0640879581285,16.4693477444567));
#10379=CARTESIAN_POINT('Ctrl Pts',(-3.87336343711624,18.8961655481765,16.4224727444567));
#10380=CARTESIAN_POINT('Ctrl Pts',(-3.95801143716275,18.561757480056,16.3287227444567));
#10381=CARTESIAN_POINT('Ctrl Pts',(-4.42040908392757,18.0438052570563,16.1412227444567));
#10382=CARTESIAN_POINT('Ctrl Pts',(-5.3597736327005,17.9486382462214,15.9068477444566));
#10383=CARTESIAN_POINT('Ctrl Pts',(-6.08353002861201,18.8291131546215,15.6255977444567));
#10384=CARTESIAN_POINT('Ctrl Pts',(-5.7522743312806,19.9169980729128,15.3443477444566));
#10385=CARTESIAN_POINT('Ctrl Pts',(-4.66432852032523,20.247484037686,15.0630977444567));
#10386=CARTESIAN_POINT('Ctrl Pts',(-3.7847912177152,19.5257370720338,14.7818477444566));
#10387=CARTESIAN_POINT('Ctrl Pts',(-3.89641685998538,18.3938296969161,14.5005977444567));
#10388=CARTESIAN_POINT('Ctrl Pts',(-4.8994990955269,17.8575969427705,14.2193477444567));
#10389=CARTESIAN_POINT('Ctrl Pts',(-5.90268327503555,18.3938108560019,13.9380977444567));
#10390=CARTESIAN_POINT('Ctrl Pts',(-6.01415671724292,19.5257840424613,13.6568477444567));
#10391=CARTESIAN_POINT('Ctrl Pts',(-5.13489691562506,20.2473857741269,13.3755977444567));
#10392=CARTESIAN_POINT('Ctrl Pts',(-4.04641130741378,19.9171961820093,13.0943477444566));
#10393=CARTESIAN_POINT('Ctrl Pts',(-3.71622631011187,18.8287161056785,12.8130977444567));
#10394=CARTESIAN_POINT('Ctrl Pts',(-4.43782211894507,17.949447108094,12.5318477444566));
#10395=CARTESIAN_POINT('Ctrl Pts',(-5.56980547600071,18.0609379436409,12.2505977444567));
#10396=CARTESIAN_POINT('Ctrl Pts',(-6.10599995712322,19.0640879581285,11.9693477444567));
#10397=CARTESIAN_POINT('Ctrl Pts',(-5.56980547600071,20.0672379726161,11.6880977444567));
#10398=CARTESIAN_POINT('Ctrl Pts',(-4.43782211894506,20.178728808163,11.4068477444567));
#10399=CARTESIAN_POINT('Ctrl Pts',(-3.71622631011187,19.2994598105785,11.1255977444567));
#10400=CARTESIAN_POINT('Ctrl Pts',(-4.04641130741377,18.2109797342477,10.8443477444567));
#10401=CARTESIAN_POINT('Ctrl Pts',(-5.13489691562506,17.8807901421302,10.5630977444567));
#10402=CARTESIAN_POINT('Ctrl Pts',(-6.01415671724291,18.6023918737957,10.2818477444567));
#10403=CARTESIAN_POINT('Ctrl Pts',(-5.90268327503556,19.7343650602551,10.0005977444567));
#10404=CARTESIAN_POINT('Ctrl Pts',(-4.89949909552691,20.2705789734865,9.71934774445667));
#10405=CARTESIAN_POINT('Ctrl Pts',(-3.89641685998539,19.7343462193409,9.43809774445665));
#10406=CARTESIAN_POINT('Ctrl Pts',(-3.78479121771519,18.6024388442232,9.15684774445666));
#10407=CARTESIAN_POINT('Ctrl Pts',(-4.66432852032523,17.8806918785709,8.87559774445665));
#10408=CARTESIAN_POINT('Ctrl Pts',(-5.75227433128059,18.2111778433442,8.59434774445666));
#10409=CARTESIAN_POINT('Ctrl Pts',(-6.08353002861201,19.2990627616355,8.31309774445665));
#10410=CARTESIAN_POINT('Ctrl Pts',(-5.3597736327005,20.1795376700355,8.03184774445666));
#10411=CARTESIAN_POINT('Ctrl Pts',(-4.42040908392757,20.0843706592008,7.79747274445665));
#10412=CARTESIAN_POINT('Ctrl Pts',(-3.95801143716276,19.566418436201,7.60997274445666));
#10413=CARTESIAN_POINT('Ctrl Pts',(-3.87336343711624,19.2320103680805,7.51622274445666));
#10414=CARTESIAN_POINT('Ctrl Pts',(-3.87336343711624,19.0640879581285,7.46934774445666));
#10415=CARTESIAN_POINT('Ctrl Pts',(-3.7933878804808,19.0640879581285,16.3896597660693));
#10416=CARTESIAN_POINT('Ctrl Pts',(-3.7933878804808,18.8831088802229,16.3427847660693));
#10417=CARTESIAN_POINT('Ctrl Pts',(-3.88464146291,18.5225999274217,16.2490347660693));
#10418=CARTESIAN_POINT('Ctrl Pts',(-4.38305093345958,17.964328938091,16.0615347660693));
#10419=CARTESIAN_POINT('Ctrl Pts',(-5.39565132779325,17.8616979064182,15.8271597660693));
#10420=CARTESIAN_POINT('Ctrl Pts',(-6.17579055836198,18.8108104241486,15.5459097660693));
#10421=CARTESIAN_POINT('Ctrl Pts',(-5.81872962019059,19.9834587251169,15.2646597660693));
#10422=CARTESIAN_POINT('Ctrl Pts',(-4.64599918882846,20.3397045914162,14.9834097660693));
#10423=CARTESIAN_POINT('Ctrl Pts',(-3.69792432335972,19.5617109755361,14.7021597660693));
#10424=CARTESIAN_POINT('Ctrl Pts',(-3.81824754138906,18.3415989967109,14.4209097660693));
#10425=CARTESIAN_POINT('Ctrl Pts',(-4.89949750810393,17.7635784564526,14.1396597660693));
#10426=CARTESIAN_POINT('Ctrl Pts',(-5.98085655102714,18.3415783016242,13.8584097660693));
#10427=CARTESIAN_POINT('Ctrl Pts',(-6.10101692072211,19.5617625684221,13.5771597660692));
#10428=CARTESIAN_POINT('Ctrl Pts',(-5.15323897079963,20.3395966574836,13.2959097660693));
#10429=CARTESIAN_POINT('Ctrl Pts',(-3.97993097761014,19.9836763312797,13.0146597660693));
#10430=CARTESIAN_POINT('Ctrl Pts',(-3.62401563614486,18.8103742911771,12.7334097660693));
#10431=CARTESIAN_POINT('Ctrl Pts',(-4.40184325151628,17.8625864851583,12.4521597660693));
#10432=CARTESIAN_POINT('Ctrl Pts',(-5.62203867225617,17.9827654726664,12.1709097660693));
#10433=CARTESIAN_POINT('Ctrl Pts',(-6.20001718473,19.0640879581285,11.8896597660693));
#10434=CARTESIAN_POINT('Ctrl Pts',(-5.62203867225618,20.1454104435907,11.6084097660693));
#10435=CARTESIAN_POINT('Ctrl Pts',(-4.40184325151628,20.2655894310987,11.3271597660693));
#10436=CARTESIAN_POINT('Ctrl Pts',(-3.62401563614487,19.31780162508,11.0459097660693));
#10437=CARTESIAN_POINT('Ctrl Pts',(-3.97993097761013,18.1444995849772,10.7646597660693));
#10438=CARTESIAN_POINT('Ctrl Pts',(-5.15323897079963,17.7885792587734,10.4834097660693));
#10439=CARTESIAN_POINT('Ctrl Pts',(-6.10101692072211,18.5664133478349,10.2021597660693));
#10440=CARTESIAN_POINT('Ctrl Pts',(-5.98085655102714,19.7865976146328,9.92090976606928));
#10441=CARTESIAN_POINT('Ctrl Pts',(-4.89949750810393,20.3645974598044,9.63965976606927));
#10442=CARTESIAN_POINT('Ctrl Pts',(-3.81824754138907,19.7865769195461,9.35840976606927));
#10443=CARTESIAN_POINT('Ctrl Pts',(-3.69792432335971,18.5664649407209,9.07715976606927));
#10444=CARTESIAN_POINT('Ctrl Pts',(-4.64599918882847,17.7884713248408,8.79590976606928));
#10445=CARTESIAN_POINT('Ctrl Pts',(-5.81872962019059,18.1447171911401,8.51465976606927));
#10446=CARTESIAN_POINT('Ctrl Pts',(-6.17579055836198,19.3173654921084,8.23340976606927));
#10447=CARTESIAN_POINT('Ctrl Pts',(-5.39565132779325,20.2664780098388,7.95215976606927));
#10448=CARTESIAN_POINT('Ctrl Pts',(-4.38305093345958,20.163846978166,7.71778476606926));
#10449=CARTESIAN_POINT('Ctrl Pts',(-3.88464146291,19.6055759888353,7.53028476606928));
#10450=CARTESIAN_POINT('Ctrl Pts',(-3.7933878804808,19.2450670360341,7.43653476606927));
#10451=CARTESIAN_POINT('Ctrl Pts',(-3.7933878804808,19.0640879581285,7.38965976606927));
#10452=CARTESIAN_POINT('Ctrl Pts',(-3.68970367081301,19.0640879581285,16.3393281946845));
#10453=CARTESIAN_POINT('Ctrl Pts',(-3.68970367081301,18.8661279362491,16.2924531946845));
#10454=CARTESIAN_POINT('Ctrl Pts',(-3.78950639275064,18.4718472718449,16.1987031946845));
#10455=CARTESIAN_POINT('Ctrl Pts',(-4.33464880408738,17.8612197308254,16.0112031946845));
#10456=CARTESIAN_POINT('Ctrl Pts',(-5.44215248298708,17.7489941707718,15.7768281946845));
#10457=CARTESIAN_POINT('Ctrl Pts',(-6.29543194791065,18.7870635687412,15.4955781946845));
#10458=CARTESIAN_POINT('Ctrl Pts',(-5.90489522616153,20.069643379945,15.2143281946845));
#10459=CARTESIAN_POINT('Ctrl Pts',(-4.62223458959786,20.4592806298484,14.9330781946845));
#10460=CARTESIAN_POINT('Ctrl Pts',(-3.58528538365352,19.6083590506333,14.6518281946845));
#10461=CARTESIAN_POINT('Ctrl Pts',(-3.71688836785426,18.2738721170015,14.3705781946845));
#10462=CARTESIAN_POINT('Ctrl Pts',(-4.89949513369314,17.6416679685783,14.0893281946845));
#10463=CARTESIAN_POINT('Ctrl Pts',(-6.08222164389359,18.2738496926538,13.8080781946845));
#10464=CARTESIAN_POINT('Ctrl Pts',(-6.21364585244353,19.6084149545679,13.5268281946845));
#10465=CARTESIAN_POINT('Ctrl Pts',(-5.17702260178661,20.4591636770942,13.2455781946845));
#10466=CARTESIAN_POINT('Ctrl Pts',(-3.89372791469413,20.0698791686619,12.9643281946845));
#10467=CARTESIAN_POINT('Ctrl Pts',(-3.50444884087783,18.7865909980945,12.6830781946845));
#10468=CARTESIAN_POINT('Ctrl Pts',(-4.35519053162382,17.7499569365869,12.4018281946845));
#10469=CARTESIAN_POINT('Ctrl Pts',(-5.68976788890187,17.8814015796806,12.1205781946845));
#10470=CARTESIAN_POINT('Ctrl Pts',(-6.32192649143762,19.0640879581285,11.8393281946845));
#10471=CARTESIAN_POINT('Ctrl Pts',(-5.68976788890188,20.2467743365765,11.5580781946845));
#10472=CARTESIAN_POINT('Ctrl Pts',(-4.35519053162381,20.37821897967,11.2768281946845));
#10473=CARTESIAN_POINT('Ctrl Pts',(-3.50444884087783,19.3415849181625,10.9955781946845));
#10474=CARTESIAN_POINT('Ctrl Pts',(-3.89372791469413,18.0582967475951,10.7143281946845));
#10475=CARTESIAN_POINT('Ctrl Pts',(-5.1770226017866,17.6690122391628,10.4330781946845));
#10476=CARTESIAN_POINT('Ctrl Pts',(-6.21364585244354,18.5197609616891,10.1518281946845));
#10477=CARTESIAN_POINT('Ctrl Pts',(-6.08222164389357,19.8543262236032,9.87057819468449));
#10478=CARTESIAN_POINT('Ctrl Pts',(-4.89949513369316,20.4865079476786,9.58932819468449));
#10479=CARTESIAN_POINT('Ctrl Pts',(-3.71688836785425,19.8543037992555,9.3080781946845));
#10480=CARTESIAN_POINT('Ctrl Pts',(-3.58528538365353,18.5198168656236,9.02682819468449));
#10481=CARTESIAN_POINT('Ctrl Pts',(-4.62223458959785,17.6688952864086,8.7455781946845));
#10482=CARTESIAN_POINT('Ctrl Pts',(-5.90489522616153,18.058532536312,8.46432819468449));
#10483=CARTESIAN_POINT('Ctrl Pts',(-6.29543194791065,19.3411123475158,8.18307819468449));
#10484=CARTESIAN_POINT('Ctrl Pts',(-5.44215248298707,20.3791817454852,7.9018281946845));
#10485=CARTESIAN_POINT('Ctrl Pts',(-4.33464880408739,20.2669561854316,7.66745319468449));
#10486=CARTESIAN_POINT('Ctrl Pts',(-3.78950639275065,19.6563286444121,7.47995319468449));
#10487=CARTESIAN_POINT('Ctrl Pts',(-3.68970367081301,19.2620479800079,7.3862031946845));
#10488=CARTESIAN_POINT('Ctrl Pts',(-3.68970367081301,19.0640879581285,7.33932819468449));
#10489=CARTESIAN_POINT('Ctrl Pts',(-3.53279534926847,19.0640879581285,16.3570658392427));
#10490=CARTESIAN_POINT('Ctrl Pts',(-3.53279534926847,18.8404597227958,16.3101908392427));
#10491=CARTESIAN_POINT('Ctrl Pts',(-3.64554380498313,18.3950345896878,16.2164408392427));
#10492=CARTESIAN_POINT('Ctrl Pts',(-4.26138349750937,17.7052213564393,16.0289408392427));
#10493=CARTESIAN_POINT('Ctrl Pts',(-5.51253087910551,17.5784308548572,15.7945658392427));
#10494=CARTESIAN_POINT('Ctrl Pts',(-6.47647202312581,18.7511368435749,15.5133158392427));
#10495=CARTESIAN_POINT('Ctrl Pts',(-6.03528677810603,20.2000570979724,15.2320658392427));
#10496=CARTESIAN_POINT('Ctrl Pts',(-4.58627179173248,20.6402292551834,14.9508158392427));
#10497=CARTESIAN_POINT('Ctrl Pts',(-3.41483687900195,19.6789475644362,14.6695658392427));
#10498=CARTESIAN_POINT('Ctrl Pts',(-3.56350776503963,18.1713859243031,14.3883158392427));
#10499=CARTESIAN_POINT('Ctrl Pts',(-4.89949171467019,17.4571884927796,14.1070658392427));
#10500=CARTESIAN_POINT('Ctrl Pts',(-6.23561077022493,18.1713605115216,13.8258158392427));
#10501=CARTESIAN_POINT('Ctrl Pts',(-6.38407994614382,19.6790109185417,13.5445658392427));
#10502=CARTESIAN_POINT('Ctrl Pts',(-5.21301280428764,20.6400967164316,13.2633158392427));
#10503=CARTESIAN_POINT('Ctrl Pts',(-3.76328242757296,20.200324309785,12.9820658392427));
#10504=CARTESIAN_POINT('Ctrl Pts',(-3.32351616699498,18.7506012926997,12.7008158392427));
#10505=CARTESIAN_POINT('Ctrl Pts',(-4.28459400258271,17.5795219496166,12.4195658392427));
#10506=CARTESIAN_POINT('Ctrl Pts',(-5.79225811327219,17.7280141831339,12.1383158392427));
#10507=CARTESIAN_POINT('Ctrl Pts',(-6.50640393154715,19.0640879581285,11.8570658392427));
#10508=CARTESIAN_POINT('Ctrl Pts',(-5.79225811327219,20.4001617331231,11.5758158392427));
#10509=CARTESIAN_POINT('Ctrl Pts',(-4.28459400258271,20.5486539666404,11.2945658392427));
#10510=CARTESIAN_POINT('Ctrl Pts',(-3.32351616699498,19.3775746235574,11.0133158392427));
#10511=CARTESIAN_POINT('Ctrl Pts',(-3.76328242757296,17.9278516064719,10.7320658392427));
#10512=CARTESIAN_POINT('Ctrl Pts',(-5.21301280428765,17.4880791998254,10.4508158392427));
#10513=CARTESIAN_POINT('Ctrl Pts',(-6.38407994614382,18.4491649977153,10.1695658392427));
#10514=CARTESIAN_POINT('Ctrl Pts',(-6.23561077022493,19.9568154047354,9.88831583924269));
#10515=CARTESIAN_POINT('Ctrl Pts',(-4.89949171467019,20.6709874234774,9.60706583924272));
#10516=CARTESIAN_POINT('Ctrl Pts',(-3.56350776503964,19.9567899919539,9.32581583924268));
#10517=CARTESIAN_POINT('Ctrl Pts',(-3.41483687900194,18.4492283518208,9.04456583924271));
#10518=CARTESIAN_POINT('Ctrl Pts',(-4.58627179173249,17.4879466610736,8.76331583924269));
#10519=CARTESIAN_POINT('Ctrl Pts',(-6.03528677810602,17.9281188182846,8.48206583924271));
#10520=CARTESIAN_POINT('Ctrl Pts',(-6.47647202312581,19.3770390726821,8.20081583924271));
#10521=CARTESIAN_POINT('Ctrl Pts',(-5.51253087910551,20.5497450613998,7.91956583924269));
#10522=CARTESIAN_POINT('Ctrl Pts',(-4.26138349750937,20.4229545598178,7.68519083924271));
#10523=CARTESIAN_POINT('Ctrl Pts',(-3.64554380498314,19.7331413265693,7.4976908392427));
#10524=CARTESIAN_POINT('Ctrl Pts',(-3.53279534926847,19.2877161934612,7.4039408392427));
#10525=CARTESIAN_POINT('Ctrl Pts',(-3.53279534926847,19.0640879581285,7.3570658392427));
#10526=CARTESIAN_POINT('Ctrl Pts',(-3.39185052109767,19.0640879581285,16.4968382100706));
#10527=CARTESIAN_POINT('Ctrl Pts',(-3.39185052109767,18.8174025726682,16.4499632100706));
#10528=CARTESIAN_POINT('Ctrl Pts',(-3.51622754236571,18.326036742358,16.3562132100706));
#10529=CARTESIAN_POINT('Ctrl Pts',(-4.19557224327097,17.565093412113,16.1687132100707));
#10530=CARTESIAN_POINT('Ctrl Pts',(-5.575749054425,17.4252203273698,15.9343382100706));
#10531=CARTESIAN_POINT('Ctrl Pts',(-6.63909370032394,18.7188650976713,15.6530882100707));
#10532=CARTESIAN_POINT('Ctrl Pts',(-6.15241265775512,20.3172029701892,15.3718382100706));
#10533=CARTESIAN_POINT('Ctrl Pts',(-4.55396775605188,20.8027686951522,15.0905882100707));
#10534=CARTESIAN_POINT('Ctrl Pts',(-3.26172927687774,19.7423546302722,14.8093382100706));
#10535=CARTESIAN_POINT('Ctrl Pts',(-3.42573164117171,18.0793263581647,14.5280882100707));
#10536=CARTESIAN_POINT('Ctrl Pts',(-4.899488641356,17.2914773992253,14.2468382100707));
#10537=CARTESIAN_POINT('Ctrl Pts',(-6.37339455576845,18.0792982655374,13.9655882100707));
#10538=CARTESIAN_POINT('Ctrl Pts',(-6.53717459445583,19.7424246652384,13.6843382100706));
#10539=CARTESIAN_POINT('Ctrl Pts',(-5.24534147363094,20.8026221798253,13.4030882100707));
#10540=CARTESIAN_POINT('Ctrl Pts',(-3.64610806630185,20.3174983603167,13.1218382100707));
#10541=CARTESIAN_POINT('Ctrl Pts',(-3.16099103155741,18.7182730700627,12.8405882100707));
#10542=CARTESIAN_POINT('Ctrl Pts',(-4.2211797490425,17.4264264984208,12.5593382100707));
#10543=CARTESIAN_POINT('Ctrl Pts',(-5.88432129484326,17.5902319524447,12.2780882100707));
#10544=CARTESIAN_POINT('Ctrl Pts',(-6.67211319955942,19.0640879581285,11.9968382100707));
#10545=CARTESIAN_POINT('Ctrl Pts',(-5.88432129484326,20.5379439638123,11.7155882100707));
#10546=CARTESIAN_POINT('Ctrl Pts',(-4.2211797490425,20.7017494178361,11.4343382100706));
#10547=CARTESIAN_POINT('Ctrl Pts',(-3.16099103155741,19.4099028461943,11.1530882100707));
#10548=CARTESIAN_POINT('Ctrl Pts',(-3.64610806630184,17.8106775559402,10.8718382100706));
#10549=CARTESIAN_POINT('Ctrl Pts',(-5.24534147363094,17.3255537364318,10.5905882100707));
#10550=CARTESIAN_POINT('Ctrl Pts',(-6.53717459445584,18.3857512510185,10.3093382100707));
#10551=CARTESIAN_POINT('Ctrl Pts',(-6.37339455576845,20.0488776507196,10.0280882100707));
#10552=CARTESIAN_POINT('Ctrl Pts',(-4.89948864135601,20.8366985170317,9.74683821007065));
#10553=CARTESIAN_POINT('Ctrl Pts',(-3.42573164117171,20.0488495580922,9.46558821007067));
#10554=CARTESIAN_POINT('Ctrl Pts',(-3.26172927687774,18.3858212859848,9.18433821007065));
#10555=CARTESIAN_POINT('Ctrl Pts',(-4.55396775605187,17.3254072211048,8.90308821007067));
#10556=CARTESIAN_POINT('Ctrl Pts',(-6.15241265775512,17.8109729460678,8.62183821007066));
#10557=CARTESIAN_POINT('Ctrl Pts',(-6.63909370032395,19.4093108185857,8.34058821007066));
#10558=CARTESIAN_POINT('Ctrl Pts',(-5.575749054425,20.7029555888872,8.05933821007067));
#10559=CARTESIAN_POINT('Ctrl Pts',(-4.19557224327098,20.563082504144,7.82496321007066));
#10560=CARTESIAN_POINT('Ctrl Pts',(-3.51622754236572,19.8021391738989,7.63746321007066));
#10561=CARTESIAN_POINT('Ctrl Pts',(-3.39185052109767,19.3107733435888,7.54371321007066));
#10562=CARTESIAN_POINT('Ctrl Pts',(-3.39185052109767,19.0640879581285,7.49683821007066));
#10563=CARTESIAN_POINT('Ctrl Pts',(-3.39169248787219,19.0640879581285,16.7239302794826));
#10564=CARTESIAN_POINT('Ctrl Pts',(-3.39169248787219,18.8173582841831,16.6770552794826));
#10565=CARTESIAN_POINT('Ctrl Pts',(-3.51607750948594,18.3259638826828,16.5833052794826));
#10566=CARTESIAN_POINT('Ctrl Pts',(-4.1955090373622,17.5649114699112,16.3958052794825));
#10567=CARTESIAN_POINT('Ctrl Pts',(-5.57581566285176,17.4250519637791,16.1614302794825));
#10568=CARTESIAN_POINT('Ctrl Pts',(-6.63928646631149,18.7188226227733,15.8801802794826));
#10569=CARTESIAN_POINT('Ctrl Pts',(-6.15254732826514,20.3173418200787,15.5989302794826));
#10570=CARTESIAN_POINT('Ctrl Pts',(-4.55393099911422,20.8029567209829,15.3176802794826));
#10571=CARTESIAN_POINT('Ctrl Pts',(-3.2615505733002,19.7424290768571,15.0364302794825));
#10572=CARTESIAN_POINT('Ctrl Pts',(-3.42557143558259,18.0792188569332,14.7551802794826));
#10573=CARTESIAN_POINT('Ctrl Pts',(-4.89948852917189,17.2912846067797,14.4739302794825));
#10574=CARTESIAN_POINT('Ctrl Pts',(-6.37355504102926,18.0791909931369,14.1926802794826));
#10575=CARTESIAN_POINT('Ctrl Pts',(-6.53735282518174,19.7424985413448,13.9114302794825));
#10576=CARTESIAN_POINT('Ctrl Pts',(-5.24537912980387,20.8028113991441,13.6301802794826));
#10577=CARTESIAN_POINT('Ctrl Pts',(-3.64597162556245,20.3176348036352,13.3489302794825));
#10578=CARTESIAN_POINT('Ctrl Pts',(-3.16080179641243,18.7182354232864,13.0676802794826));
#10579=CARTESIAN_POINT('Ctrl Pts',(-4.22110590981088,17.4262482416907,12.7864302794826));
#10580=CARTESIAN_POINT('Ctrl Pts',(-5.88442849114239,17.5900715226153,12.5051802794825));
#10581=CARTESIAN_POINT('Ctrl Pts',(-6.67230614484835,19.0640879581285,12.2239302794825));
#10582=CARTESIAN_POINT('Ctrl Pts',(-5.88442849114239,20.5381043936417,11.9426802794826));
#10583=CARTESIAN_POINT('Ctrl Pts',(-4.22110590981089,20.7019276745664,11.6614302794825));
#10584=CARTESIAN_POINT('Ctrl Pts',(-3.16080179641243,19.4099404929707,11.3801802794826));
#10585=CARTESIAN_POINT('Ctrl Pts',(-3.64597162556246,17.8105411126219,11.0989302794825));
#10586=CARTESIAN_POINT('Ctrl Pts',(-5.24537912980387,17.3253645171128,10.8176802794826));
#10587=CARTESIAN_POINT('Ctrl Pts',(-6.53735282518174,18.3856773749122,10.5364302794826));
#10588=CARTESIAN_POINT('Ctrl Pts',(-6.37355504102926,20.0489849231201,10.2551802794825));
#10589=CARTESIAN_POINT('Ctrl Pts',(-4.8994885291719,20.8368913094773,9.97393027948256));
#10590=CARTESIAN_POINT('Ctrl Pts',(-3.42557143558259,20.0489570593238,9.69268027948254));
#10591=CARTESIAN_POINT('Ctrl Pts',(-3.2615505733002,18.3857468394,9.41143027948255));
#10592=CARTESIAN_POINT('Ctrl Pts',(-4.55393099911421,17.3252191952741,9.13018027948254));
#10593=CARTESIAN_POINT('Ctrl Pts',(-6.15254732826515,17.8108340961783,8.84893027948254));
#10594=CARTESIAN_POINT('Ctrl Pts',(-6.63928646631149,19.4093532934837,8.56768027948255));
#10595=CARTESIAN_POINT('Ctrl Pts',(-5.57581566285176,20.7031239524779,8.28643027948254));
#10596=CARTESIAN_POINT('Ctrl Pts',(-4.19550903736219,20.5632644463458,8.05205527948254));
#10597=CARTESIAN_POINT('Ctrl Pts',(-3.51607750948594,19.8022120335742,7.86455527948255));
#10598=CARTESIAN_POINT('Ctrl Pts',(-3.39169248787219,19.3108176320739,7.77080527948255));
#10599=CARTESIAN_POINT('Ctrl Pts',(-3.39169248787219,19.0640879581285,7.72393027948255));
#10600=CARTESIAN_POINT('Ctrl Pts',(-3.58586566110283,19.0640879581285,16.8792307126044));
#10601=CARTESIAN_POINT('Ctrl Pts',(-3.58586566110283,18.8491619105832,16.8323557126044));
#10602=CARTESIAN_POINT('Ctrl Pts',(-3.69424116423088,18.4210095347625,16.7386057126044));
#10603=CARTESIAN_POINT('Ctrl Pts',(-4.28615185108811,17.7580115827766,16.5511057126044));
#10604=CARTESIAN_POINT('Ctrl Pts',(-5.48873191468298,17.6361158104589,16.3167307126044));
#10605=CARTESIAN_POINT('Ctrl Pts',(-6.41522812207474,18.7632951732742,16.0354807126044));
#10606=CARTESIAN_POINT('Ctrl Pts',(-5.99118137092013,20.1559395583845,15.7542307126044));
#10607=CARTESIAN_POINT('Ctrl Pts',(-4.59843590585757,20.5790214675252,15.4729807126044));
#10608=CARTESIAN_POINT('Ctrl Pts',(-3.4724946609971,19.6550690290813,15.1917307126044));
#10609=CARTESIAN_POINT('Ctrl Pts',(-3.61539129834037,18.2060540861185,14.9104807126044));
#10610=CARTESIAN_POINT('Ctrl Pts',(-4.89949299231913,17.5195918519191,14.6292307126044));
#10611=CARTESIAN_POINT('Ctrl Pts',(-6.18372405178529,18.2060294255882,14.3479807126044));
#10612=CARTESIAN_POINT('Ctrl Pts',(-6.3264275493564,19.6551305078257,14.0667307126044));
#10613=CARTESIAN_POINT('Ctrl Pts',(-5.20083844932418,20.5788928520569,13.7854807126044));
#10614=CARTESIAN_POINT('Ctrl Pts',(-3.80740799028661,20.1561988608322,13.5042307126044));
#10615=CARTESIAN_POINT('Ctrl Pts',(-3.38471992582087,18.7627754696101,13.2229807126044));
#10616=CARTESIAN_POINT('Ctrl Pts',(-4.30847456266717,17.6371746765229,12.9417307126044));
#10617=CARTESIAN_POINT('Ctrl Pts',(-5.75758893238404,17.7799002566516,12.6604807126044));
#10618=CARTESIAN_POINT('Ctrl Pts',(-6.44400108821606,19.0640879581285,12.3792307126044));
#10619=CARTESIAN_POINT('Ctrl Pts',(-5.75758893238404,20.3482756596054,12.0979807126044));
#10620=CARTESIAN_POINT('Ctrl Pts',(-4.30847456266717,20.4910012397341,11.8167307126044));
#10621=CARTESIAN_POINT('Ctrl Pts',(-3.38471992582088,19.3654004466468,11.5354807126044));
#10622=CARTESIAN_POINT('Ctrl Pts',(-3.8074079902866,17.9719770554247,11.2542307126044));
#10623=CARTESIAN_POINT('Ctrl Pts',(-5.20083844932418,17.5492830642001,10.9729807126044));
#10624=CARTESIAN_POINT('Ctrl Pts',(-6.3264275493564,18.4730454084312,10.6917307126044));
#10625=CARTESIAN_POINT('Ctrl Pts',(-6.18372405178529,19.9221464906688,10.4104807126044));
#10626=CARTESIAN_POINT('Ctrl Pts',(-4.89949299231914,20.6085840643379,10.1292307126044));
#10627=CARTESIAN_POINT('Ctrl Pts',(-3.61539129834038,19.9221218301385,9.84798071260441));
#10628=CARTESIAN_POINT('Ctrl Pts',(-3.4724946609971,18.4731068871757,9.56673071260441));
#10629=CARTESIAN_POINT('Ctrl Pts',(-4.59843590585757,17.5491544487319,9.28548071260441));
#10630=CARTESIAN_POINT('Ctrl Pts',(-5.99118137092013,17.9722363578725,9.00423071260441));
#10631=CARTESIAN_POINT('Ctrl Pts',(-6.41522812207474,19.3648807429828,8.72298071260441));
#10632=CARTESIAN_POINT('Ctrl Pts',(-5.48873191468298,20.4920601057981,8.44173071260441));
#10633=CARTESIAN_POINT('Ctrl Pts',(-4.28615185108811,20.3701643334804,8.20735571260441));
#10634=CARTESIAN_POINT('Ctrl Pts',(-3.69424116423088,19.7071663814945,8.01985571260441));
#10635=CARTESIAN_POINT('Ctrl Pts',(-3.58586566110283,19.2790140056738,7.92610571260441));
#10636=CARTESIAN_POINT('Ctrl Pts',(-3.58586566110283,19.0640879581285,7.87923071260441));
#10637=CARTESIAN_POINT('Ctrl Pts',(-3.82796762890525,19.0640879581285,16.823577010191));
#10638=CARTESIAN_POINT('Ctrl Pts',(-3.82796762890525,18.8887036859235,16.776702010191));
#10639=CARTESIAN_POINT('Ctrl Pts',(-3.91635126240454,18.5395431958975,16.682952010191));
#10640=CARTESIAN_POINT('Ctrl Pts',(-4.39923287559051,17.9986246601018,16.495452010191));
#10641=CARTESIAN_POINT('Ctrl Pts',(-5.3801268299794,17.8992984782641,16.261077010191));
#10642=CARTESIAN_POINT('Ctrl Pts',(-6.13592767953631,18.81870686685,15.979827010191));
#10643=CARTESIAN_POINT('Ctrl Pts',(-5.79000493363568,19.9547431341663,15.698577010191));
#10644=CARTESIAN_POINT('Ctrl Pts',(-4.65392293358042,20.299846234605,15.417327010191));
#10645=CARTESIAN_POINT('Ctrl Pts',(-3.73546442954298,19.546165820423,15.136077010191));
#10646=CARTESIAN_POINT('Ctrl Pts',(-3.85203058955701,18.3641706998376,14.854827010191));
#10647=CARTESIAN_POINT('Ctrl Pts',(-4.89949789588871,17.8042108777981,14.573577010191));
#10648=CARTESIAN_POINT('Ctrl Pts',(-5.94707253612464,18.3641514430527,14.292327010191));
#10649=CARTESIAN_POINT('Ctrl Pts',(-6.06347844901485,19.5462138276125,14.011077010191));
#10650=CARTESIAN_POINT('Ctrl Pts',(-5.14531211795937,20.299745802162,13.729827010191));
#10651=CARTESIAN_POINT('Ctrl Pts',(-4.0086617797242,19.9549456152629,13.448577010191));
#10652=CARTESIAN_POINT('Ctrl Pts',(-3.66386635646435,18.818301064382,13.167327010191));
#10653=CARTESIAN_POINT('Ctrl Pts',(-4.41739224278398,17.9001250692965,12.886077010191));
#10654=CARTESIAN_POINT('Ctrl Pts',(-5.59946504144651,18.0165492869179,12.604827010191));
#10655=CARTESIAN_POINT('Ctrl Pts',(-6.1593857329367,19.0640879581285,12.323577010191));
#10656=CARTESIAN_POINT('Ctrl Pts',(-5.59946504144652,20.1116266293391,12.042327010191));
#10657=CARTESIAN_POINT('Ctrl Pts',(-4.41739224278398,20.2280508469605,11.761077010191));
#10658=CARTESIAN_POINT('Ctrl Pts',(-3.66386635646435,19.3098748518751,11.479827010191));
#10659=CARTESIAN_POINT('Ctrl Pts',(-4.0086617797242,18.173230300994,11.198577010191));
#10660=CARTESIAN_POINT('Ctrl Pts',(-5.14531211795937,17.828430114095,10.917327010191));
#10661=CARTESIAN_POINT('Ctrl Pts',(-6.06347844901484,18.5819620886445,10.636077010191));
#10662=CARTESIAN_POINT('Ctrl Pts',(-5.94707253612464,19.7640244732043,10.354827010191));
#10663=CARTESIAN_POINT('Ctrl Pts',(-4.89949789588871,20.3239650384589,10.073577010191));
#10664=CARTESIAN_POINT('Ctrl Pts',(-3.85203058955702,19.7640052164194,9.792327010191));
#10665=CARTESIAN_POINT('Ctrl Pts',(-3.73546442954297,18.582010095834,9.51107701019101));
#10666=CARTESIAN_POINT('Ctrl Pts',(-4.65392293358042,17.8283296816519,9.22982701019099));
#10667=CARTESIAN_POINT('Ctrl Pts',(-5.79000493363569,18.1734327820907,8.94857701019101));
#10668=CARTESIAN_POINT('Ctrl Pts',(-6.1359276795363,19.309469049407,8.667327010191));
#10669=CARTESIAN_POINT('Ctrl Pts',(-5.38012682997942,20.2288774379929,8.38607701019101));
#10670=CARTESIAN_POINT('Ctrl Pts',(-4.3992328755905,20.1295512561551,8.15170201019099));
#10671=CARTESIAN_POINT('Ctrl Pts',(-3.91635126240454,19.5886327203595,7.96420201019101));
#10672=CARTESIAN_POINT('Ctrl Pts',(-3.82796762890525,19.2394722303336,7.870452010191));
#10673=CARTESIAN_POINT('Ctrl Pts',(-3.82796762890525,19.0640879581285,7.82357701019101));
#10674=CARTESIAN_POINT('Ctrl Pts',(-3.89952178519528,19.0640879581285,16.6747998250855));
#10675=CARTESIAN_POINT('Ctrl Pts',(-3.89952178519528,18.9005833965992,16.6279248250855));
#10676=CARTESIAN_POINT('Ctrl Pts',(-3.98204948501551,18.57452912557,16.5341748250855));
#10677=CARTESIAN_POINT('Ctrl Pts',(-4.43254360294575,18.069998639348,16.3466748250855));
#10678=CARTESIAN_POINT('Ctrl Pts',(-5.34807292990168,17.9770472888948,16.1122998250855));
#10679=CARTESIAN_POINT('Ctrl Pts',(-6.05327021347282,18.8351498528125,15.8310498250855));
#10680=CARTESIAN_POINT('Ctrl Pts',(-5.73051146706618,19.8952002447694,15.5497998250855));
#10681=CARTESIAN_POINT('Ctrl Pts',(-4.67032794951053,20.2172744300372,15.2685498250855));
#10682=CARTESIAN_POINT('Ctrl Pts',(-3.81325976534224,19.5139439749143,14.9872998250854));
#10683=CARTESIAN_POINT('Ctrl Pts',(-3.92203016364069,18.4109474713839,14.7060498250855));
#10684=CARTESIAN_POINT('Ctrl Pts',(-4.89950048344233,17.8884042869319,14.4247998250854));
#10685=CARTESIAN_POINT('Ctrl Pts',(-5.87706651134918,18.4109273848096,14.1435498250855));
#10686=CARTESIAN_POINT('Ctrl Pts',(-5.98569401960982,19.513994050791,13.8622998250855));
#10687=CARTESIAN_POINT('Ctrl Pts',(-5.12888636151304,20.2171696695614,13.5810498250855));
#10688=CARTESIAN_POINT('Ctrl Pts',(-4.06819606995765,19.8954114551267,13.2997998250855));
#10689=CARTESIAN_POINT('Ctrl Pts',(-3.74644247556127,18.8347265100042,13.0185498250855));
#10690=CARTESIAN_POINT('Ctrl Pts',(-4.44961192317263,17.9779101434778,12.7372998250855));
#10691=CARTESIAN_POINT('Ctrl Pts',(-5.55268935359726,18.0865540151131,12.4560498250855));
#10692=CARTESIAN_POINT('Ctrl Pts',(-6.07519178725272,19.0640879581285,12.1747998250855));
#10693=CARTESIAN_POINT('Ctrl Pts',(-5.55268935359726,20.041621901144,11.8935498250855));
#10694=CARTESIAN_POINT('Ctrl Pts',(-4.44961192317262,20.1502657727792,11.6122998250855));
#10695=CARTESIAN_POINT('Ctrl Pts',(-3.74644247556128,19.2934494062529,11.3310498250855));
#10696=CARTESIAN_POINT('Ctrl Pts',(-4.06819606995765,18.2327644611302,11.0497998250855));
#10697=CARTESIAN_POINT('Ctrl Pts',(-5.12888636151305,17.9110062466957,10.7685498250855));
#10698=CARTESIAN_POINT('Ctrl Pts',(-5.98569401960981,18.614181865466,10.4872998250855));
#10699=CARTESIAN_POINT('Ctrl Pts',(-5.87706651134917,19.7172485314474,10.2060498250855));
#10700=CARTESIAN_POINT('Ctrl Pts',(-4.89950048344233,20.2397716293251,9.92479982508547));
#10701=CARTESIAN_POINT('Ctrl Pts',(-3.92203016364069,19.7172284448732,9.64354982508546));
#10702=CARTESIAN_POINT('Ctrl Pts',(-3.81325976534224,18.6142319413427,9.36229982508548));
#10703=CARTESIAN_POINT('Ctrl Pts',(-4.67032794951052,17.9109014862198,9.08104982508547));
#10704=CARTESIAN_POINT('Ctrl Pts',(-5.73051146706617,18.2329756714876,8.79979982508548));
#10705=CARTESIAN_POINT('Ctrl Pts',(-6.05327021347282,19.2930260634445,8.51854982508547));
#10706=CARTESIAN_POINT('Ctrl Pts',(-5.34807292990168,20.1511286273622,8.23729982508547));
#10707=CARTESIAN_POINT('Ctrl Pts',(-4.43254360294574,20.0581772769091,8.00292482508547));
#10708=CARTESIAN_POINT('Ctrl Pts',(-3.98204948501552,19.553646790687,7.81542482508548));
#10709=CARTESIAN_POINT('Ctrl Pts',(-3.89952178519528,19.2275925196578,7.72167482508547));
#10710=CARTESIAN_POINT('Ctrl Pts',(-3.89952178519528,19.0640879581285,7.67479982508547));
#10711=CARTESIAN_POINT('Ctrl Pts',(-3.89952178519528,19.0640879581285,16.6));
#10712=CARTESIAN_POINT('Ctrl Pts',(-3.89952178519528,18.900463340754,16.553125));
#10713=CARTESIAN_POINT('Ctrl Pts',(-3.98201667654796,18.574558453354,16.459375));
#10714=CARTESIAN_POINT('Ctrl Pts',(-4.43261252959751,18.0698369774179,16.271875));
#10715=CARTESIAN_POINT('Ctrl Pts',(-5.3480450944344,17.9770695761824,16.0375));
#10716=CARTESIAN_POINT('Ctrl Pts',(-6.05333812005169,18.8351088887249,15.75625));
#10717=CARTESIAN_POINT('Ctrl Pts',(-5.73053324403457,19.8952490922453,15.475));
#10718=CARTESIAN_POINT('Ctrl Pts',(-4.67032445705031,20.2173120687642,15.19375));
#10719=CARTESIAN_POINT('Ctrl Pts',(-3.81321396620606,19.5139658030124,14.9125));
#10720=CARTESIAN_POINT('Ctrl Pts',(-3.92199288032869,18.4109195983283,14.63125));
#10721=CARTESIAN_POINT('Ctrl Pts',(-4.89949977532975,17.8883587658141,14.35));
#10722=CARTESIAN_POINT('Ctrl Pts',(-5.87710555996492,18.4109010214894,14.06875));
#10723=CARTESIAN_POINT('Ctrl Pts',(-5.98573683407846,19.5140121151019,13.7875));
#10724=CARTESIAN_POINT('Ctrl Pts',(-5.1288955300064,20.2172151824403,13.50625));
#10725=CARTESIAN_POINT('Ctrl Pts',(-4.06816311909486,19.8954444250534,13.225));
#10726=CARTESIAN_POINT('Ctrl Pts',(-3.74639685722716,18.8347173994404,12.94375));
#10727=CARTESIAN_POINT('Ctrl Pts',(-4.44959410269395,17.9778671655289,12.6625));
#10728=CARTESIAN_POINT('Ctrl Pts',(-5.55271521450753,18.0865153161182,12.38125));
#10729=CARTESIAN_POINT('Ctrl Pts',(-6.07523831702883,19.0640879581285,12.1));
#10730=CARTESIAN_POINT('Ctrl Pts',(-5.55271521450754,20.0416606001388,11.81875));
#10731=CARTESIAN_POINT('Ctrl Pts',(-4.44959410269395,20.1503087507281,11.5375));
#10732=CARTESIAN_POINT('Ctrl Pts',(-3.74639685722716,19.2934585168167,11.25625));
#10733=CARTESIAN_POINT('Ctrl Pts',(-4.06816311909486,18.2327314912035,10.975));
#10734=CARTESIAN_POINT('Ctrl Pts',(-5.12889553000641,17.9109607338168,10.69375));
#10735=CARTESIAN_POINT('Ctrl Pts',(-5.98573683407846,18.6141638011551,10.4125));
#10736=CARTESIAN_POINT('Ctrl Pts',(-5.87710555996491,19.7172748947676,10.13125));
#10737=CARTESIAN_POINT('Ctrl Pts',(-4.89949977532976,20.2398171504429,9.84999999999999));
#10738=CARTESIAN_POINT('Ctrl Pts',(-3.92199288032869,19.7172563179287,9.56875000000001));
#10739=CARTESIAN_POINT('Ctrl Pts',(-3.81321396620606,18.6142101132445,9.2875));
#10740=CARTESIAN_POINT('Ctrl Pts',(-4.67032445705031,17.9108638474928,9.00625));
#10741=CARTESIAN_POINT('Ctrl Pts',(-5.73053324403456,18.2329268240116,8.725));
#10742=CARTESIAN_POINT('Ctrl Pts',(-6.05333812005169,19.2930670275321,8.44375));
#10743=CARTESIAN_POINT('Ctrl Pts',(-5.34804509443441,20.1511063400746,8.1625));
#10744=CARTESIAN_POINT('Ctrl Pts',(-4.43261252959751,20.0583389388391,7.928125));
#10745=CARTESIAN_POINT('Ctrl Pts',(-3.98201667654797,19.553617462903,7.740625));
#10746=CARTESIAN_POINT('Ctrl Pts',(-3.89952178519528,19.227712575503,7.646875));
#10747=CARTESIAN_POINT('Ctrl Pts',(-3.89952178519528,19.0640879581285,7.6));
#10748=CARTESIAN_POINT('',(-3.89952178519528,19.0640879581285,7.6));
#10749=CARTESIAN_POINT('Ctrl Pts',(-3.89952178519528,19.0640879581285,16.6));
#10750=CARTESIAN_POINT('Ctrl Pts',(-3.89952178519528,18.900463340754,16.553125));
#10751=CARTESIAN_POINT('Ctrl Pts',(-3.98201667654796,18.574558453354,16.459375));
#10752=CARTESIAN_POINT('Ctrl Pts',(-4.43261252959751,18.0698369774179,16.271875));
#10753=CARTESIAN_POINT('Ctrl Pts',(-5.3480450944344,17.9770695761824,16.0375));
#10754=CARTESIAN_POINT('Ctrl Pts',(-6.05333812005169,18.8351088887249,15.75625));
#10755=CARTESIAN_POINT('Ctrl Pts',(-5.73053324403457,19.8952490922453,15.475));
#10756=CARTESIAN_POINT('Ctrl Pts',(-4.67032445705031,20.2173120687642,15.19375));
#10757=CARTESIAN_POINT('Ctrl Pts',(-3.81321396620606,19.5139658030124,14.9125));
#10758=CARTESIAN_POINT('Ctrl Pts',(-3.92199288032869,18.4109195983283,14.63125));
#10759=CARTESIAN_POINT('Ctrl Pts',(-4.89949977532975,17.8883587658141,14.35));
#10760=CARTESIAN_POINT('Ctrl Pts',(-5.87710555996492,18.4109010214894,14.06875));
#10761=CARTESIAN_POINT('Ctrl Pts',(-5.98573683407846,19.5140121151019,13.7875));
#10762=CARTESIAN_POINT('Ctrl Pts',(-5.1288955300064,20.2172151824403,13.50625));
#10763=CARTESIAN_POINT('Ctrl Pts',(-4.06816311909486,19.8954444250534,13.225));
#10764=CARTESIAN_POINT('Ctrl Pts',(-3.74639685722716,18.8347173994404,12.94375));
#10765=CARTESIAN_POINT('Ctrl Pts',(-4.44959410269395,17.9778671655289,12.6625));
#10766=CARTESIAN_POINT('Ctrl Pts',(-5.55271521450753,18.0865153161182,12.38125));
#10767=CARTESIAN_POINT('Ctrl Pts',(-6.07523831702883,19.0640879581285,12.1));
#10768=CARTESIAN_POINT('Ctrl Pts',(-5.55271521450754,20.0416606001388,11.81875));
#10769=CARTESIAN_POINT('Ctrl Pts',(-4.44959410269395,20.1503087507281,11.5375));
#10770=CARTESIAN_POINT('Ctrl Pts',(-3.74639685722716,19.2934585168167,11.25625));
#10771=CARTESIAN_POINT('Ctrl Pts',(-4.06816311909486,18.2327314912035,10.975));
#10772=CARTESIAN_POINT('Ctrl Pts',(-5.12889553000641,17.9109607338168,10.69375));
#10773=CARTESIAN_POINT('Ctrl Pts',(-5.98573683407846,18.6141638011551,10.4125));
#10774=CARTESIAN_POINT('Ctrl Pts',(-5.87710555996491,19.7172748947676,10.13125));
#10775=CARTESIAN_POINT('Ctrl Pts',(-4.89949977532976,20.2398171504429,9.84999999999999));
#10776=CARTESIAN_POINT('Ctrl Pts',(-3.92199288032869,19.7172563179287,9.56875000000001));
#10777=CARTESIAN_POINT('Ctrl Pts',(-3.81321396620606,18.6142101132445,9.2875));
#10778=CARTESIAN_POINT('Ctrl Pts',(-4.67032445705031,17.9108638474928,9.00625));
#10779=CARTESIAN_POINT('Ctrl Pts',(-5.73053324403456,18.2329268240116,8.725));
#10780=CARTESIAN_POINT('Ctrl Pts',(-6.05333812005169,19.2930670275321,8.44375));
#10781=CARTESIAN_POINT('Ctrl Pts',(-5.34804509443441,20.1511063400746,8.1625));
#10782=CARTESIAN_POINT('Ctrl Pts',(-4.43261252959751,20.0583389388391,7.928125));
#10783=CARTESIAN_POINT('Ctrl Pts',(-3.98201667654797,19.553617462903,7.740625));
#10784=CARTESIAN_POINT('Ctrl Pts',(-3.89952178519528,19.227712575503,7.646875));
#10785=CARTESIAN_POINT('Ctrl Pts',(-3.89952178519528,19.0640879581285,7.6));
#10786=CARTESIAN_POINT('Origin',(-3.64952178519528,19.0640879581285,7.6));
#10787=CARTESIAN_POINT('Origin',(-3.64952178519528,19.0640879581285,7.6));
#10788=CARTESIAN_POINT('',(0.,0.,0.));
#10789=CARTESIAN_POINT('Origin',(-18.7359120418715,27.7504782148047,17.6));
#10790=CARTESIAN_POINT('',(-18.0859120418715,27.8004782148047,17.6));
#10791=CARTESIAN_POINT('Origin',(-18.7359120418715,27.8004782148047,17.6));
#10792=CARTESIAN_POINT('',(-17.9859120418715,27.7004782148047,17.6));
#10793=CARTESIAN_POINT('',(-18.0359120418715,27.7504782148047,17.6));
#10794=CARTESIAN_POINT('Origin',(-18.7359120418715,27.7004782148047,17.6));
#10795=CARTESIAN_POINT('Origin',(-18.7359120418715,22.4004782148047,17.6));
#10796=CARTESIAN_POINT('',(-17.9859120418715,22.5004782148047,17.6));
#10797=CARTESIAN_POINT('',(-17.9859120418715,22.4004782148047,17.6));
#10798=CARTESIAN_POINT('Origin',(-18.7359120418715,22.5004782148047,17.6));
#10799=CARTESIAN_POINT('Origin',(-18.7359120418715,27.8004782148047,17.6));
#10800=CARTESIAN_POINT('Origin',(-18.7359120418715,22.4504782148047,17.6));
#10801=CARTESIAN_POINT('',(-18.0859120418715,22.4004782148047,17.6));
#10802=CARTESIAN_POINT('',(-18.0359120418715,22.4504782148047,17.6));
#10803=CARTESIAN_POINT('Origin',(-18.7359120418715,22.4004782148047,17.6));
#10804=CARTESIAN_POINT('Origin',(-18.7359120418715,22.4004782148047,17.6));
#10805=CARTESIAN_POINT('',(0.,0.,0.));
#10806=CARTESIAN_POINT('Origin',(-18.7359120418715,26.3504782148047,17.6));
#10807=CARTESIAN_POINT('',(-18.7359120418715,26.3504782148047,18.35));
#10808=CARTESIAN_POINT('Origin',(-18.7359120418715,26.3504782148047,18.6));
#10809=CARTESIAN_POINT('Origin',(-18.7359120418715,26.3504782148047,17.6));
#10810=CARTESIAN_POINT('',(-18.7359120418715,26.6004782148047,16.6));
#10811=CARTESIAN_POINT('',(-18.7359120418715,26.1004782148047,16.6));
#10812=CARTESIAN_POINT('Origin',(-18.7359120418715,26.3504782148047,16.6));
#10813=CARTESIAN_POINT('Ctrl Pts',(-18.7359120418715,26.6004782148047,16.6));
#10814=CARTESIAN_POINT('Ctrl Pts',(-18.7402193353539,26.6004782148047,16.5977092724426));
#10815=CARTESIAN_POINT('Ctrl Pts',(-18.7445589464746,26.6004467587024,16.5954788663774));
#10816=CARTESIAN_POINT('Ctrl Pts',(-18.7872540124717,26.5998563522904,16.5742560748851));
#10817=CARTESIAN_POINT('Ctrl Pts',(-18.8283064246552,26.5971771315259,16.559542959919));
#10818=CARTESIAN_POINT('Ctrl Pts',(-18.8701108612612,26.5930900009076,16.5481972195909));
#10819=CARTESIAN_POINT('Ctrl Pts',(-18.8708339684841,26.5930188703742,16.5480020646239));
#10820=CARTESIAN_POINT('Ctrl Pts',(-18.8827759229911,26.5918370097103,16.544797109728));
#10821=CARTESIAN_POINT('Ctrl Pts',(-18.894063293504,26.590615824153,16.5420298581508));
#10822=CARTESIAN_POINT('Ctrl Pts',(-18.910070277255,26.5887362807543,16.5384418503857));
#10823=CARTESIAN_POINT('Ctrl Pts',(-18.9147727349573,26.5881661562854,16.5374286265409));
#10824=CARTESIAN_POINT('Ctrl Pts',(-18.9230847074372,26.5871263380585,16.5357072275207));
#10825=CARTESIAN_POINT('Ctrl Pts',(-18.9266932353496,26.5866642710644,16.5349829852478));
#10826=CARTESIAN_POINT('Ctrl Pts',(-18.9343464784642,26.585661455081,16.5334946079531));
#10827=CARTESIAN_POINT('Ctrl Pts',(-18.9383928290144,26.5851177664648,16.5327358435474));
#10828=CARTESIAN_POINT('Ctrl Pts',(-18.9481733797635,26.5837704893605,16.5309679692519));
#10829=CARTESIAN_POINT('Ctrl Pts',(-18.9539124540547,26.5829524731398,16.5299854641958));
#10830=CARTESIAN_POINT('Ctrl Pts',(-18.9737387918633,26.5800291593595,16.5267739133408));
#10831=CARTESIAN_POINT('Ctrl Pts',(-18.9878669666236,26.577776425181,16.5248034466825));
#10832=CARTESIAN_POINT('Ctrl Pts',(-19.0400872187947,26.568769854808,16.5186110231589));
#10833=CARTESIAN_POINT('Ctrl Pts',(-19.0785053382042,26.5608013780416,16.5162061142361));
#10834=CARTESIAN_POINT('Ctrl Pts',(-19.1413563804704,26.5448431161272,16.5154725363415));
#10835=CARTESIAN_POINT('Ctrl Pts',(-19.1663341463412,26.5377137973801,16.5160451884648));
#10836=CARTESIAN_POINT('Ctrl Pts',(-19.2675067236831,26.5048705240401,16.5219235534991));
#10837=CARTESIAN_POINT('Ctrl Pts',(-19.3339527175624,26.4736908333921,16.5341985199053));
#10838=CARTESIAN_POINT('Ctrl Pts',(-19.4275973319121,26.408664050569,16.5639151059098));
#10839=CARTESIAN_POINT('Ctrl Pts',(-19.4584745098273,26.3779628401158,16.5791986989673));
#10840=CARTESIAN_POINT('Ctrl Pts',(-19.493043062557,26.3250017138209,16.605627659773));
#10841=CARTESIAN_POINT('Ctrl Pts',(-19.5019011653722,26.3029596082007,16.6166575639151));
#10842=CARTESIAN_POINT('Ctrl Pts',(-19.5077448592175,26.2652062478922,16.6350648852536));
#10843=CARTESIAN_POINT('Ctrl Pts',(-19.5070741798815,26.2486012355754,16.6429988757827));
#10844=CARTESIAN_POINT('Ctrl Pts',(-19.498268450351,26.2180039204305,16.6569651923278));
#10845=CARTESIAN_POINT('Ctrl Pts',(-19.4911945436197,26.2046479601392,16.6627780404676));
#10846=CARTESIAN_POINT('Ctrl Pts',(-19.4706730422176,26.17894609994,16.6732083185761));
#10847=CARTESIAN_POINT('Ctrl Pts',(-19.4571316130369,26.1675135294197,16.677362768157));
#10848=CARTESIAN_POINT('Ctrl Pts',(-19.4199753453774,26.1438724951594,16.6848437491615));
#10849=CARTESIAN_POINT('Ctrl Pts',(-19.3946921404572,26.1337519058654,16.686910649375));
#10850=CARTESIAN_POINT('Ctrl Pts',(-19.3217072854985,26.1124320719796,16.6888104810606));
#10851=CARTESIAN_POINT('Ctrl Pts',(-19.2671883817412,26.1060347853434,16.6853604690573));
#10852=CARTESIAN_POINT('Ctrl Pts',(-19.0981182229277,26.0969290280957,16.6690502405298));
#10853=CARTESIAN_POINT('Ctrl Pts',(-18.8857203861473,26.1008383327785,16.6427595546923));
#10854=CARTESIAN_POINT('Ctrl Pts',(-18.741103632581,26.1004816814786,16.6015112866721));
#10855=CARTESIAN_POINT('Ctrl Pts',(-18.7385065750259,26.1004782148047,16.6007604391535));
#10856=CARTESIAN_POINT('Ctrl Pts',(-18.7359120418715,26.1004782148047,16.6));
#10857=CARTESIAN_POINT('Ctrl Pts',(-18.7359120418715,26.1004782148047,16.6));
#10858=CARTESIAN_POINT('Ctrl Pts',(-18.899536659246,26.1004782148047,16.553125));
#10859=CARTESIAN_POINT('Ctrl Pts',(-19.2254952210856,26.0179991230989,16.459375));
#10860=CARTESIAN_POINT('Ctrl Pts',(-19.7300373474021,25.5673218790664,16.271875));
#10861=CARTESIAN_POINT('Ctrl Pts',(-19.8229633788124,24.6519659680192,16.0375));
#10862=CARTESIAN_POINT('Ctrl Pts',(-18.9648841528132,23.9466522306267,15.75625));
#10863=CARTESIAN_POINT('Ctrl Pts',(-17.9047456459512,24.2694552701876,15.475));
#10864=CARTESIAN_POINT('Ctrl Pts',(-17.5826797074142,25.3296825136249,15.19375));
#10865=CARTESIAN_POINT('Ctrl Pts',(-18.2860294065758,26.1867906898977,14.9125));
#10866=CARTESIAN_POINT('Ctrl Pts',(-19.389086573694,26.0780174976981,14.63125));
#10867=CARTESIAN_POINT('Ctrl Pts',(-19.9116498391532,25.1004985660911,14.35));
#10868=CARTESIAN_POINT('Ctrl Pts',(-19.3891045896494,24.1228877031823,14.06875));
#10869=CARTESIAN_POINT('Ctrl Pts',(-18.2859840561,24.0142539916667,13.7875));
#10870=CARTESIAN_POINT('Ctrl Pts',(-17.582775853732,24.8711029879984,13.50625));
#10871=CARTESIAN_POINT('Ctrl Pts',(-17.9045489079489,25.9318432698064,13.225));
#10872=CARTESIAN_POINT('Ctrl Pts',(-18.9652844651045,26.2536123707356,12.94375));
#10873=CARTESIAN_POINT('Ctrl Pts',(-19.8221414011456,25.5504093950162,12.6625));
#10874=CARTESIAN_POINT('Ctrl Pts',(-19.7134924282747,24.4472796581219,12.38125));
#10875=CARTESIAN_POINT('Ctrl Pts',(-18.7359120418715,23.9247523488297,12.1));
#10876=CARTESIAN_POINT('Ctrl Pts',(-17.7583316554683,24.4472796581219,11.81875));
#10877=CARTESIAN_POINT('Ctrl Pts',(-17.6496826825974,25.5504093950162,11.5375));
#10878=CARTESIAN_POINT('Ctrl Pts',(-18.5065396186384,26.2536123707357,11.25625));
#10879=CARTESIAN_POINT('Ctrl Pts',(-19.567275175794,25.9318432698063,10.975));
#10880=CARTESIAN_POINT('Ctrl Pts',(-19.8890482300109,24.8711029879984,10.69375));
#10881=CARTESIAN_POINT('Ctrl Pts',(-19.185840027643,24.0142539916666,10.4125));
#10882=CARTESIAN_POINT('Ctrl Pts',(-18.0827194940936,24.1228877031824,10.13125));
#10883=CARTESIAN_POINT('Ctrl Pts',(-17.5601742445898,25.1004985660911,9.85));
#10884=CARTESIAN_POINT('Ctrl Pts',(-18.082737510049,26.0780174976981,9.56875));
#10885=CARTESIAN_POINT('Ctrl Pts',(-19.1857946771672,26.1867906898977,9.2875));
#10886=CARTESIAN_POINT('Ctrl Pts',(-19.8891443763288,25.329682513625,9.00625));
#10887=CARTESIAN_POINT('Ctrl Pts',(-19.5670784377918,24.2694552701875,8.725));
#10888=CARTESIAN_POINT('Ctrl Pts',(-18.5069399309298,23.9466522306267,8.44375));
#10889=CARTESIAN_POINT('Ctrl Pts',(-17.6488607049306,24.6519659680192,8.16250000000001));
#10890=CARTESIAN_POINT('Ctrl Pts',(-17.7417867363409,25.5673218790663,7.928125));
#10891=CARTESIAN_POINT('Ctrl Pts',(-18.2463288626574,26.0179991230989,7.740625));
#10892=CARTESIAN_POINT('Ctrl Pts',(-18.572287424497,26.1004782148047,7.646875));
#10893=CARTESIAN_POINT('Ctrl Pts',(-18.7359120418715,26.1004782148047,7.6));
#10894=CARTESIAN_POINT('Ctrl Pts',(-18.7359120418715,26.1004782148047,16.5252001749145));
#10895=CARTESIAN_POINT('Ctrl Pts',(-18.8994338407553,26.1004782148047,16.4783251749145));
#10896=CARTESIAN_POINT('Ctrl Pts',(-19.2255030930883,26.0179660342054,16.3845751749145));
#10897=CARTESIAN_POINT('Ctrl Pts',(-19.729867953292,25.5673943129456,16.1970751749145));
#10898=CARTESIAN_POINT('Ctrl Pts',(-19.8229695302986,24.6519424250744,15.9627001749145));
#10899=CARTESIAN_POINT('Ctrl Pts',(-18.9648436629017,23.9467315923973,15.6814501749145));
#10900=CARTESIAN_POINT('Ctrl Pts',(-17.9048011394298,24.2694854426487,15.4002001749145));
#10901=CARTESIAN_POINT('Ctrl Pts',(-17.5827296870337,25.3296765835496,15.1189501749145));
#10902=CARTESIAN_POINT('Ctrl Pts',(-18.2860551788254,26.1867342513203,14.8377001749145));
#10903=CARTESIAN_POINT('Ctrl Pts',(-19.3890525137468,26.0779704411713,14.5564501749145));
#10904=CARTESIAN_POINT('Ctrl Pts',(-19.9115925078101,25.1004979111444,14.2752001749145));
#10905=CARTESIAN_POINT('Ctrl Pts',(-19.3890718388655,24.1229364083568,13.9939501749145));
#10906=CARTESIAN_POINT('Ctrl Pts',(-18.2860065328672,24.0143075901023,13.7127001749145));
#10907=CARTESIAN_POINT('Ctrl Pts',(-17.582832820097,24.8711144190662,13.4314501749145));
#10908=CARTESIAN_POINT('Ctrl Pts',(-17.9045901039069,25.9318020855622,13.1502001749145));
#10909=CARTESIAN_POINT('Ctrl Pts',(-18.9652730883107,26.2535553206106,12.8689501749145));
#10910=CARTESIAN_POINT('Ctrl Pts',(-19.8220876543766,25.550387117378,12.5877001749145));
#10911=CARTESIAN_POINT('Ctrl Pts',(-19.7134440422139,24.4473119914142,12.3064501749145));
#10912=CARTESIAN_POINT('Ctrl Pts',(-18.7359120418715,23.9248105319629,12.0252001749145));
#10913=CARTESIAN_POINT('Ctrl Pts',(-17.7583800415291,24.4473119914142,11.7439501749145));
#10914=CARTESIAN_POINT('Ctrl Pts',(-17.6497364293663,25.550387117378,11.4627001749145));
#10915=CARTESIAN_POINT('Ctrl Pts',(-18.5065509954323,26.2535553206107,11.1814501749145));
#10916=CARTESIAN_POINT('Ctrl Pts',(-19.567233979836,25.9318020855621,10.9002001749145));
#10917=CARTESIAN_POINT('Ctrl Pts',(-19.888991263646,24.8711144190662,10.6189501749145));
#10918=CARTESIAN_POINT('Ctrl Pts',(-19.1858175508758,24.0143075901023,10.3377001749145));
#10919=CARTESIAN_POINT('Ctrl Pts',(-18.0827522448775,24.1229364083568,10.0564501749145));
#10920=CARTESIAN_POINT('Ctrl Pts',(-17.5602315759329,25.1004979111444,9.77520017491453));
#10921=CARTESIAN_POINT('Ctrl Pts',(-18.0827715699962,26.0779704411713,9.49395017491453));
#10922=CARTESIAN_POINT('Ctrl Pts',(-19.1857689049176,26.1867342513203,9.21270017491453));
#10923=CARTESIAN_POINT('Ctrl Pts',(-19.8890943967093,25.3296765835496,8.93145017491453));
#10924=CARTESIAN_POINT('Ctrl Pts',(-19.5670229443132,24.2694854426487,8.65020017491453));
#10925=CARTESIAN_POINT('Ctrl Pts',(-18.5069804208413,23.9467315923973,8.36895017491453));
#10926=CARTESIAN_POINT('Ctrl Pts',(-17.6488545534444,24.6519424250744,8.08770017491453));
#10927=CARTESIAN_POINT('Ctrl Pts',(-17.741956130451,25.5673943129456,7.85332517491453));
#10928=CARTESIAN_POINT('Ctrl Pts',(-18.2463209906547,26.0179660342054,7.66582517491453));
#10929=CARTESIAN_POINT('Ctrl Pts',(-18.5723902429877,26.1004782148047,7.57207517491453));
#10930=CARTESIAN_POINT('Ctrl Pts',(-18.7359120418715,26.1004782148047,7.52520017491453));
#10931=CARTESIAN_POINT('Ctrl Pts',(-18.7359120418715,26.1719704380264,16.3763120970567));
#10932=CARTESIAN_POINT('Ctrl Pts',(-18.9112832567962,26.1719704380264,16.3294370970567));
#10933=CARTESIAN_POINT('Ctrl Pts',(-19.2604928816873,26.0836104084264,16.2356870970568));
#10934=CARTESIAN_POINT('Ctrl Pts',(-19.8011898254895,25.6006632552387,16.0481870970567));
#10935=CARTESIAN_POINT('Ctrl Pts',(-19.9006761814027,24.6199119837374,15.8138120970568));
#10936=CARTESIAN_POINT('Ctrl Pts',(-18.9812730600262,23.8641250484612,15.5325620970567));
#10937=CARTESIAN_POINT('Ctrl Pts',(-17.8452974226091,24.2100292982365,15.2513120970568));
#10938=CARTESIAN_POINT('Ctrl Pts',(-17.5002088862725,25.3460716478709,14.9700620970567));
#10939=CARTESIAN_POINT('Ctrl Pts',(-18.2538540872815,26.2644803214233,14.6888120970568));
#10940=CARTESIAN_POINT('Ctrl Pts',(-19.4357996089,26.1479262471745,14.4075620970567));
#10941=CARTESIAN_POINT('Ctrl Pts',(-19.9957331087188,25.1005003313284,14.1263120970567));
#10942=CARTESIAN_POINT('Ctrl Pts',(-19.4358182926448,24.0529745102095,13.8450620970567));
#10943=CARTESIAN_POINT('Ctrl Pts',(-18.2538070558221,23.9365720149762,13.5638120970568));
#10944=CARTESIAN_POINT('Ctrl Pts',(-17.5003085963596,24.8546990276559,13.2825620970567));
#10945=CARTESIAN_POINT('Ctrl Pts',(-17.8450933927673,25.9912989167809,13.0013120970568));
#10946=CARTESIAN_POINT('Ctrl Pts',(-18.9816881993013,26.3360795225021,12.7200620970567));
#10947=CARTESIAN_POINT('Ctrl Pts',(-19.899823815302,25.5825865293351,12.4388120970567));
#10948=CARTESIAN_POINT('Ctrl Pts',(-19.7834047461942,24.4005657233216,12.1575620970567));
#10949=CARTESIAN_POINT('Ctrl Pts',(-18.7359120418715,23.8406695287272,11.8763120970567));
#10950=CARTESIAN_POINT('Ctrl Pts',(-17.6884193375488,24.4005657233217,11.5950620970567));
#10951=CARTESIAN_POINT('Ctrl Pts',(-17.5720002684409,25.582586529335,11.3138120970567));
#10952=CARTESIAN_POINT('Ctrl Pts',(-18.4901358844417,26.3360795225021,11.0325620970568));
#10953=CARTESIAN_POINT('Ctrl Pts',(-19.6267306909757,25.9912989167809,10.7513120970567));
#10954=CARTESIAN_POINT('Ctrl Pts',(-19.9715154873835,24.8546990276559,10.4700620970567));
#10955=CARTESIAN_POINT('Ctrl Pts',(-19.2180170279209,23.9365720149762,10.1888120970567));
#10956=CARTESIAN_POINT('Ctrl Pts',(-18.0360057910981,24.0529745102095,9.90756209705675));
#10957=CARTESIAN_POINT('Ctrl Pts',(-17.4760909750243,25.1005003313284,9.62631209705675));
#10958=CARTESIAN_POINT('Ctrl Pts',(-18.036024474843,26.1479262471745,9.34506209705674));
#10959=CARTESIAN_POINT('Ctrl Pts',(-19.2179699964615,26.2644803214233,9.06381209705675));
#10960=CARTESIAN_POINT('Ctrl Pts',(-19.9716151974705,25.3460716478709,8.78256209705674));
#10961=CARTESIAN_POINT('Ctrl Pts',(-19.6265266611339,24.2100292982365,8.50131209705674));
#10962=CARTESIAN_POINT('Ctrl Pts',(-18.4905510237168,23.8641250484612,8.22006209705674));
#10963=CARTESIAN_POINT('Ctrl Pts',(-17.5711479023404,24.6199119837374,7.93881209705675));
#10964=CARTESIAN_POINT('Ctrl Pts',(-17.6706342582534,25.6006632552387,7.70443709705674));
#10965=CARTESIAN_POINT('Ctrl Pts',(-18.2113312020557,26.0836104084263,7.51693709705675));
#10966=CARTESIAN_POINT('Ctrl Pts',(-18.5605408269468,26.1719704380264,7.42318709705674));
#10967=CARTESIAN_POINT('Ctrl Pts',(-18.7359120418715,26.1719704380264,7.37631209705674));
#10968=CARTESIAN_POINT('Ctrl Pts',(-18.7359120418715,26.4141284002705,16.3210712807239));
#10969=CARTESIAN_POINT('Ctrl Pts',(-18.9508421867125,26.4141284002705,16.2741962807239));
#10970=CARTESIAN_POINT('Ctrl Pts',(-19.3790542523568,26.305774781696,16.1804462807239));
#10971=CARTESIAN_POINT('Ctrl Pts',(-20.0418196213741,25.7137583047068,15.9929462807239));
#10972=CARTESIAN_POINT('Ctrl Pts',(-20.1639181514686,24.5112865006198,15.7585712807239));
#10973=CARTESIAN_POINT('Ctrl Pts',(-19.0366952474877,23.5847663556869,15.4773212807239));
#10974=CARTESIAN_POINT('Ctrl Pts',(-17.6440584440828,24.008809278139,15.1960712807239));
#10975=CARTESIAN_POINT('Ctrl Pts',(-17.220975640258,25.401571598331,14.9148212807239));
#10976=CARTESIAN_POINT('Ctrl Pts',(-18.1449274857128,26.5275043655938,14.6335712807239));
#10977=CARTESIAN_POINT('Ctrl Pts',(-19.5939497971795,26.3846158434426,14.3523212807239));
#10978=CARTESIAN_POINT('Ctrl Pts',(-20.2804116503335,25.1005048514074,14.0710712807239));
#10979=CARTESIAN_POINT('Ctrl Pts',(-19.5939736594703,23.8162735358942,13.7898212807239));
#10980=CARTESIAN_POINT('Ctrl Pts',(-18.1448674186095,23.6735675718114,13.5085712807239));
#10981=CARTESIAN_POINT('Ctrl Pts',(-17.2211029869125,24.7991611137086,13.2273212807239));
#10982=CARTESIAN_POINT('Ctrl Pts',(-17.6437978626977,26.1925949193548,12.9460712807239));
#10983=CARTESIAN_POINT('Ctrl Pts',(-19.0372254681633,26.6152845876365,12.6648212807239));
#10984=CARTESIAN_POINT('Ctrl Pts',(-20.1628294097853,25.6915270641991,12.3835712807239));
#10985=CARTESIAN_POINT('Ctrl Pts',(-20.0201034674711,24.2424086412214,12.1023212807239));
#10986=CARTESIAN_POINT('Ctrl Pts',(-18.7359120418715,23.5559944071884,11.8210712807239));
#10987=CARTESIAN_POINT('Ctrl Pts',(-17.451720616272,24.2424086412214,11.5398212807239));
#10988=CARTESIAN_POINT('Ctrl Pts',(-17.3089946739576,25.6915270641991,11.2585712807239));
#10989=CARTESIAN_POINT('Ctrl Pts',(-18.4345986155797,26.6152845876365,10.9773212807239));
#10990=CARTESIAN_POINT('Ctrl Pts',(-19.8280262210453,26.1925949193548,10.6960712807239));
#10991=CARTESIAN_POINT('Ctrl Pts',(-20.2507210968305,24.7991611137086,10.4148212807239));
#10992=CARTESIAN_POINT('Ctrl Pts',(-19.3269566651335,23.6735675718114,10.1335712807239));
#10993=CARTESIAN_POINT('Ctrl Pts',(-17.8778504242727,23.8162735358942,9.8523212807239));
#10994=CARTESIAN_POINT('Ctrl Pts',(-17.1914124334094,25.1005048514074,9.5710712807239));
#10995=CARTESIAN_POINT('Ctrl Pts',(-17.8778742865635,26.3846158434426,9.28982128072389));
#10996=CARTESIAN_POINT('Ctrl Pts',(-19.3268965980302,26.5275043655938,9.00857128072391));
#10997=CARTESIAN_POINT('Ctrl Pts',(-20.250848443485,25.401571598331,8.72732128072388));
#10998=CARTESIAN_POINT('Ctrl Pts',(-19.8277656396602,24.008809278139,8.44607128072391));
#10999=CARTESIAN_POINT('Ctrl Pts',(-18.4351288362553,23.5847663556869,8.16482128072388));
#11000=CARTESIAN_POINT('Ctrl Pts',(-17.3079059322744,24.5112865006198,7.88357128072391));
#11001=CARTESIAN_POINT('Ctrl Pts',(-17.4300044623689,25.7137583047068,7.6491962807239));
#11002=CARTESIAN_POINT('Ctrl Pts',(-18.0927698313862,26.305774781696,7.4616962807239));
#11003=CARTESIAN_POINT('Ctrl Pts',(-18.5209818970305,26.4141284002705,7.3679462807239));
#11004=CARTESIAN_POINT('Ctrl Pts',(-18.7359120418715,26.4141284002705,7.3210712807239));
#11005=CARTESIAN_POINT('Ctrl Pts',(-18.7359120418715,26.6084571633498,16.4758041204314));
#11006=CARTESIAN_POINT('Ctrl Pts',(-18.9826469033796,26.6084571633498,16.4289291204314));
#11007=CARTESIAN_POINT('Ctrl Pts',(-19.4741937528585,26.4840779780848,16.3351791204314));
#11008=CARTESIAN_POINT('Ctrl Pts',(-20.2350195258441,25.8044739987892,16.1476791204314));
#11009=CARTESIAN_POINT('Ctrl Pts',(-20.375163029678,24.4241294443889,15.9133041204314));
#11010=CARTESIAN_POINT('Ctrl Pts',(-19.0811941654188,23.3605387996255,15.6320541204314));
#11011=CARTESIAN_POINT('Ctrl Pts',(-17.4825347251303,23.8473153437877,15.3508041204314));
#11012=CARTESIAN_POINT('Ctrl Pts',(-16.9968656612976,25.4461130330323,15.0695541204314));
#11013=CARTESIAN_POINT('Ctrl Pts',(-18.0575004077785,26.7386103777278,14.7883041204314));
#11014=CARTESIAN_POINT('Ctrl Pts',(-19.7208829623709,26.5745833887618,14.5070541204314));
#11015=CARTESIAN_POINT('Ctrl Pts',(-20.5088956419845,25.1005088555967,14.2258041204314));
#11016=CARTESIAN_POINT('Ctrl Pts',(-19.7209102270372,23.6262959111371,13.9445541204314));
#11017=CARTESIAN_POINT('Ctrl Pts',(-18.0574317760813,23.4624789235696,13.6633041204314));
#11018=CARTESIAN_POINT('Ctrl Pts',(-16.9970111655101,24.7545860482947,13.3820541204314));
#11019=CARTESIAN_POINT('Ctrl Pts',(-17.4822369891815,26.3541561653093,13.1008041204314));
#11020=CARTESIAN_POINT('Ctrl Pts',(-19.0817999846728,26.8393760204334,12.8195541204314));
#11021=CARTESIAN_POINT('Ctrl Pts',(-20.3739190673027,25.778963312495,12.5383041204314));
#11022=CARTESIAN_POINT('Ctrl Pts',(-20.2100791005622,24.1154709374084,12.2570541204314));
#11023=CARTESIAN_POINT('Ctrl Pts',(-18.7359120418715,23.3275126699529,11.9758041204314));
#11024=CARTESIAN_POINT('Ctrl Pts',(-17.2617449831808,24.1154709374084,11.6945541204314));
#11025=CARTESIAN_POINT('Ctrl Pts',(-17.0979050164403,25.778963312495,11.4133041204314));
#11026=CARTESIAN_POINT('Ctrl Pts',(-18.3900240990702,26.8393760204334,11.1320541204314));
#11027=CARTESIAN_POINT('Ctrl Pts',(-19.9895870945615,26.3541561653093,10.8508041204314));
#11028=CARTESIAN_POINT('Ctrl Pts',(-20.4748129182329,24.7545860482946,10.5695541204314));
#11029=CARTESIAN_POINT('Ctrl Pts',(-19.4143923076617,23.4624789235696,10.2883041204314));
#11030=CARTESIAN_POINT('Ctrl Pts',(-17.7509138567058,23.6262959111371,10.0070541204314));
#11031=CARTESIAN_POINT('Ctrl Pts',(-16.9629284417585,25.1005088555967,9.72580412043144));
#11032=CARTESIAN_POINT('Ctrl Pts',(-17.7509411213721,26.5745833887619,9.44455412043143));
#11033=CARTESIAN_POINT('Ctrl Pts',(-19.4143236759645,26.7386103777278,9.16330412043143));
#11034=CARTESIAN_POINT('Ctrl Pts',(-20.4749584224454,25.4461130330323,8.88205412043143));
#11035=CARTESIAN_POINT('Ctrl Pts',(-19.9892893586127,23.8473153437877,8.60080412043143));
#11036=CARTESIAN_POINT('Ctrl Pts',(-18.3906299183242,23.3605387996255,8.31955412043143));
#11037=CARTESIAN_POINT('Ctrl Pts',(-17.096661054065,24.4241294443889,8.03830412043144));
#11038=CARTESIAN_POINT('Ctrl Pts',(-17.2368045578989,25.8044739987892,7.80392912043142));
#11039=CARTESIAN_POINT('Ctrl Pts',(-17.9976303308845,26.4840779780847,7.61642912043144));
#11040=CARTESIAN_POINT('Ctrl Pts',(-18.4891771803634,26.6084571633498,7.52267912043143));
#11041=CARTESIAN_POINT('Ctrl Pts',(-18.7359120418715,26.6084571633498,7.47580412043143));
#11042=CARTESIAN_POINT('Ctrl Pts',(-18.7359120418715,26.6081737492155,16.7240897479859));
#11043=CARTESIAN_POINT('Ctrl Pts',(-18.9826173818796,26.6081737492155,16.6772147479859));
#11044=CARTESIAN_POINT('Ctrl Pts',(-19.4740537078383,26.4838233629858,16.5834647479859));
#11045=CARTESIAN_POINT('Ctrl Pts',(-20.2347655405055,25.8043298167281,16.3959647479859));
#11046=CARTESIAN_POINT('Ctrl Pts',(-20.3748539357312,24.4242604178057,16.1615897479859));
#11047=CARTESIAN_POINT('Ctrl Pts',(-19.0811359078137,23.360852802763,15.8803397479859));
#11048=CARTESIAN_POINT('Ctrl Pts',(-17.4827611940112,23.8475459221466,15.5990897479859));
#11049=CARTESIAN_POINT('Ctrl Pts',(-16.9971843119434,25.4460490452383,15.3178397479859));
#11050=CARTESIAN_POINT('Ctrl Pts',(-18.0576236867847,26.7383117517441,15.0365897479859));
#11051=CARTESIAN_POINT('Ctrl Pts',(-19.7207034259278,26.574314052913,14.7553397479859));
#11052=CARTESIAN_POINT('Ctrl Pts',(-20.5085718179255,25.1005089571751,14.4740897479859));
#11053=CARTESIAN_POINT('Ctrl Pts',(-19.7207304709154,23.6265649912903,14.1928397479859));
#11054=CARTESIAN_POINT('Ctrl Pts',(-18.0575556080725,23.4627779900428,13.9115897479859));
#11055=CARTESIAN_POINT('Ctrl Pts',(-16.9973286437738,24.7546491829152,13.6303397479859));
#11056=CARTESIAN_POINT('Ctrl Pts',(-17.4824658571953,26.3539272948311,13.3490897479859));
#11057=CARTESIAN_POINT('Ctrl Pts',(-19.0817368419513,26.8390585564741,13.0678397479859));
#11058=CARTESIAN_POINT('Ctrl Pts',(-20.3736200236858,25.778839446961,12.7865897479859));
#11059=CARTESIAN_POINT('Ctrl Pts',(-20.2098099709757,24.1156507636605,12.5053397479859));
#11060=CARTESIAN_POINT('Ctrl Pts',(-18.7359120418715,23.3278363510213,12.2240897479859));
#11061=CARTESIAN_POINT('Ctrl Pts',(-17.2620141127673,24.1156507636606,11.9428397479859));
#11062=CARTESIAN_POINT('Ctrl Pts',(-17.0982040600572,25.778839446961,11.6615897479859));
#11063=CARTESIAN_POINT('Ctrl Pts',(-18.3900872417917,26.8390585564741,11.3803397479859));
#11064=CARTESIAN_POINT('Ctrl Pts',(-19.9893582265476,26.3539272948311,11.0990897479859));
#11065=CARTESIAN_POINT('Ctrl Pts',(-20.4744954399692,24.7546491829153,10.8178397479859));
#11066=CARTESIAN_POINT('Ctrl Pts',(-19.4142684756705,23.4627779900428,10.5365897479859));
#11067=CARTESIAN_POINT('Ctrl Pts',(-17.7510936128276,23.6265649912903,10.2553397479859));
#11068=CARTESIAN_POINT('Ctrl Pts',(-16.9632522658175,25.1005089571751,9.97408974798591));
#11069=CARTESIAN_POINT('Ctrl Pts',(-17.7511206578151,26.574314052913,9.69283974798589));
#11070=CARTESIAN_POINT('Ctrl Pts',(-19.4142003969583,26.7383117517442,9.41158974798592));
#11071=CARTESIAN_POINT('Ctrl Pts',(-20.4746397717996,25.4460490452383,9.1303397479859));
#11072=CARTESIAN_POINT('Ctrl Pts',(-19.9890628897318,23.8475459221467,8.84908974798591));
#11073=CARTESIAN_POINT('Ctrl Pts',(-18.3906881759293,23.360852802763,8.5678397479859));
#11074=CARTESIAN_POINT('Ctrl Pts',(-17.0969701480118,24.4242604178057,8.2865897479859));
#11075=CARTESIAN_POINT('Ctrl Pts',(-17.2370585432375,25.804329816728,8.05221474798591));
#11076=CARTESIAN_POINT('Ctrl Pts',(-17.9977703759046,26.4838233629858,7.8647147479859));
#11077=CARTESIAN_POINT('Ctrl Pts',(-18.4892067018634,26.6081737492155,7.7709647479859));
#11078=CARTESIAN_POINT('Ctrl Pts',(-18.7359120418715,26.6081737492155,7.7240897479859));
#11079=CARTESIAN_POINT('Ctrl Pts',(-18.7359120418715,26.4142031825479,16.8791537727106));
#11080=CARTESIAN_POINT('Ctrl Pts',(-18.9508538798108,26.4142031825479,16.8322787727106));
#11081=CARTESIAN_POINT('Ctrl Pts',(-19.3790909060845,26.305843221212,16.7385287727106));
#11082=CARTESIAN_POINT('Ctrl Pts',(-20.0418930695294,25.7137935989603,16.5510287727106));
#11083=CARTESIAN_POINT('Ctrl Pts',(-20.1639994761375,24.5112528354905,16.3166537727106));
#11084=CARTESIAN_POINT('Ctrl Pts',(-19.0367121566617,23.5846804891688,16.0354037727106));
#11085=CARTESIAN_POINT('Ctrl Pts',(-17.6439965807029,24.0087472917322,15.7541537727107));
#11086=CARTESIAN_POINT('Ctrl Pts',(-17.2208896629275,25.4015887074258,15.4729037727106));
#11087=CARTESIAN_POINT('Ctrl Pts',(-18.1448939786028,26.5275853043863,15.1916537727106));
#11088=CARTESIAN_POINT('Ctrl Pts',(-19.5939984631419,26.3846886974873,14.9104037727106));
#11089=CARTESIAN_POINT('Ctrl Pts',(-20.2804992718394,25.1005048494697,14.6291537727106));
#11090=CARTESIAN_POINT('Ctrl Pts',(-19.5940223336954,23.8162006867272,14.3479037727106));
#11091=CARTESIAN_POINT('Ctrl Pts',(-18.1448338907002,23.673486624616,14.0666537727106));
#11092=CARTESIAN_POINT('Ctrl Pts',(-17.2210170536785,24.7991440208896,13.7854037727106));
#11093=CARTESIAN_POINT('Ctrl Pts',(-17.6437359090807,26.1926568731773,13.5041537727106));
#11094=CARTESIAN_POINT('Ctrl Pts',(-19.0372425610592,26.615370520276,13.2229037727106));
#11095=CARTESIAN_POINT('Ctrl Pts',(-20.1629103565813,25.6915605933992,12.9416537727106));
#11096=CARTESIAN_POINT('Ctrl Pts',(-20.0201763175665,24.2423599643414,12.6604037727107));
#11097=CARTESIAN_POINT('Ctrl Pts',(-18.7359120418715,23.5559067910743,12.3791537727106));
#11098=CARTESIAN_POINT('Ctrl Pts',(-17.4516477661765,24.2423599643414,12.0979037727106));
#11099=CARTESIAN_POINT('Ctrl Pts',(-17.3089137271617,25.6915605933992,11.8166537727106));
#11100=CARTESIAN_POINT('Ctrl Pts',(-18.4345815226838,26.615370520276,11.5354037727106));
#11101=CARTESIAN_POINT('Ctrl Pts',(-19.8280881746623,26.1926568731773,11.2541537727106));
#11102=CARTESIAN_POINT('Ctrl Pts',(-20.2508070300645,24.7991440208897,10.9729037727106));
#11103=CARTESIAN_POINT('Ctrl Pts',(-19.3269901930428,23.673486624616,10.6916537727106));
#11104=CARTESIAN_POINT('Ctrl Pts',(-17.8778017500476,23.8162006867272,10.4104037727106));
#11105=CARTESIAN_POINT('Ctrl Pts',(-17.1913248119037,25.1005048494697,10.1291537727106));
#11106=CARTESIAN_POINT('Ctrl Pts',(-17.8778256206011,26.3846886974873,9.84790377271063));
#11107=CARTESIAN_POINT('Ctrl Pts',(-19.3269301051402,26.5275853043863,9.56665377271064));
#11108=CARTESIAN_POINT('Ctrl Pts',(-20.2509344208154,25.4015887074258,9.28540377271063));
#11109=CARTESIAN_POINT('Ctrl Pts',(-19.8278275030402,24.0087472917322,9.00415377271064));
#11110=CARTESIAN_POINT('Ctrl Pts',(-18.4351119270813,23.5846804891688,8.72290377271064));
#11111=CARTESIAN_POINT('Ctrl Pts',(-17.3078246076055,24.5112528354905,8.44165377271065));
#11112=CARTESIAN_POINT('Ctrl Pts',(-17.4299310142136,25.7137935989603,8.20727877271063));
#11113=CARTESIAN_POINT('Ctrl Pts',(-18.0927331776585,26.3058432212119,8.01977877271064));
#11114=CARTESIAN_POINT('Ctrl Pts',(-18.5209702039323,26.4142031825479,7.92602877271064));
#11115=CARTESIAN_POINT('Ctrl Pts',(-18.7359120418715,26.4142031825479,7.87915377271064));
#11116=CARTESIAN_POINT('Ctrl Pts',(-18.7359120418715,26.1720057758739,16.8236417604652));
#11117=CARTESIAN_POINT('Ctrl Pts',(-18.9112831752672,26.1720057758739,16.7767667604652));
#11118=CARTESIAN_POINT('Ctrl Pts',(-19.2605106314382,26.0836409446025,16.6830167604652));
#11119=CARTESIAN_POINT('Ctrl Pts',(-19.8012152953036,25.6006838833452,16.4955167604651));
#11120=CARTESIAN_POINT('Ctrl Pts',(-19.9007149462722,24.6198947916415,16.2611417604652));
#11121=CARTESIAN_POINT('Ctrl Pts',(-18.9812788422948,23.8640888006839,15.9798917604651));
#11122=CARTESIAN_POINT('Ctrl Pts',(-17.8452712157343,24.21000165239,15.6986417604652));
#11123=CARTESIAN_POINT('Ctrl Pts',(-17.5001709838288,25.3460794092692,15.4173917604651));
#11124=CARTESIAN_POINT('Ctrl Pts',(-18.2538396591719,26.264515490713,15.1361417604652));
#11125=CARTESIAN_POINT('Ctrl Pts',(-19.4358207482657,26.1479581077059,14.8548917604651));
#11126=CARTESIAN_POINT('Ctrl Pts',(-19.995771387193,25.1005002946964,14.5736417604652));
#11127=CARTESIAN_POINT('Ctrl Pts',(-19.4358395073079,24.052942741889,14.2923917604651));
#11128=CARTESIAN_POINT('Ctrl Pts',(-18.2537924381707,23.9365366868337,14.0111417604652));
#11129=CARTESIAN_POINT('Ctrl Pts',(-17.500271095763,24.8546915739354,13.7298917604652));
#11130=CARTESIAN_POINT('Ctrl Pts',(-17.8450663635619,25.9913259467221,13.4486417604652));
#11131=CARTESIAN_POINT('Ctrl Pts',(-18.981695656018,26.3361170182501,13.1673917604652));
#11132=CARTESIAN_POINT('Ctrl Pts',(-19.8998591351667,25.5826011584555,12.8861417604651));
#11133=CARTESIAN_POINT('Ctrl Pts',(-19.7834365323557,24.400544484637,12.6048917604652));
#11134=CARTESIAN_POINT('Ctrl Pts',(-18.7359120418715,23.8406312992516,12.3236417604652));
#11135=CARTESIAN_POINT('Ctrl Pts',(-17.6883875513873,24.400544484637,12.0423917604652));
#11136=CARTESIAN_POINT('Ctrl Pts',(-17.5719649485763,25.5826011584555,11.7611417604651));
#11137=CARTESIAN_POINT('Ctrl Pts',(-18.490128427725,26.3361170182501,11.4798917604652));
#11138=CARTESIAN_POINT('Ctrl Pts',(-19.6267577201811,25.9913259467221,11.1986417604651));
#11139=CARTESIAN_POINT('Ctrl Pts',(-19.97155298798,24.8546915739354,10.9173917604652));
#11140=CARTESIAN_POINT('Ctrl Pts',(-19.2180316455722,23.9365366868336,10.6361417604652));
#11141=CARTESIAN_POINT('Ctrl Pts',(-18.0359845764351,24.052942741889,10.3548917604651));
#11142=CARTESIAN_POINT('Ctrl Pts',(-17.4760526965499,25.1005002946963,10.0736417604652));
#11143=CARTESIAN_POINT('Ctrl Pts',(-18.0360033354773,26.1479581077059,9.79239176046515));
#11144=CARTESIAN_POINT('Ctrl Pts',(-19.217984424571,26.264515490713,9.51114176046517));
#11145=CARTESIAN_POINT('Ctrl Pts',(-19.9716530999141,25.3460794092692,9.22989176046515));
#11146=CARTESIAN_POINT('Ctrl Pts',(-19.6265528680087,24.21000165239,8.94864176046517));
#11147=CARTESIAN_POINT('Ctrl Pts',(-18.4905452414482,23.8640888006839,8.66739176046515));
#11148=CARTESIAN_POINT('Ctrl Pts',(-17.5711091374708,24.6198947916415,8.38614176046516));
#11149=CARTESIAN_POINT('Ctrl Pts',(-17.6706087884394,25.6006838833452,8.15176676046515));
#11150=CARTESIAN_POINT('Ctrl Pts',(-18.2113134523048,26.0836409446025,7.96426676046516));
#11151=CARTESIAN_POINT('Ctrl Pts',(-18.5605409084758,26.1720057758739,7.87051676046516));
#11152=CARTESIAN_POINT('Ctrl Pts',(-18.7359120418715,26.1720057758739,7.82364176046516));
#11153=CARTESIAN_POINT('Ctrl Pts',(-18.7359120418715,26.1004782148047,16.6747998250855));
#11154=CARTESIAN_POINT('Ctrl Pts',(-18.8994244050499,26.1004782148047,16.6279248250855));
#11155=CARTESIAN_POINT('Ctrl Pts',(-19.225503815506,26.0179629976208,16.5341748250855));
#11156=CARTESIAN_POINT('Ctrl Pts',(-19.729852407908,25.5674009602397,16.3466748250855));
#11157=CARTESIAN_POINT('Ctrl Pts',(-19.8229700948236,24.6519402645263,16.1122998250855));
#11158=CARTESIAN_POINT('Ctrl Pts',(-18.9648399471218,23.9467388754675,15.8310498250855));
#11159=CARTESIAN_POINT('Ctrl Pts',(-17.9048062320946,24.2694882115908,15.5497998250855));
#11160=CARTESIAN_POINT('Ctrl Pts',(-17.5827342736889,25.3296760393435,15.2685498250855));
#11161=CARTESIAN_POINT('Ctrl Pts',(-18.2860575439579,26.1867290719232,14.9872998250855));
#11162=CARTESIAN_POINT('Ctrl Pts',(-19.389049388048,26.0779661227699,14.7060498250855));
#11163=CARTESIAN_POINT('Ctrl Pts',(-19.9115872464834,25.1004978510395,14.4247998250855));
#11164=CARTESIAN_POINT('Ctrl Pts',(-19.3890688333093,24.1229408780555,14.1435498250855));
#11165=CARTESIAN_POINT('Ctrl Pts',(-18.2860085955716,24.0143125088581,13.8622998250855));
#11166=CARTESIAN_POINT('Ctrl Pts',(-17.5828380479293,24.8711154681011,13.5810498250855));
#11167=CARTESIAN_POINT('Ctrl Pts',(-17.904593884481,25.931798306063,13.2997998250855));
#11168=CARTESIAN_POINT('Ctrl Pts',(-18.9652720442565,26.2535500850915,13.0185498250855));
#11169=CARTESIAN_POINT('Ctrl Pts',(-19.8220827220082,25.5503850729478,12.7372998250855));
#11170=CARTESIAN_POINT('Ctrl Pts',(-19.7134396018004,24.4473149586569,12.4560498250855));
#11171=CARTESIAN_POINT('Ctrl Pts',(-18.7359120418715,23.9248158714588,12.1747998250854));
#11172=CARTESIAN_POINT('Ctrl Pts',(-17.7583844819426,24.4473149586569,11.8935498250855));
#11173=CARTESIAN_POINT('Ctrl Pts',(-17.6497413617348,25.5503850729478,11.6122998250855));
#11174=CARTESIAN_POINT('Ctrl Pts',(-18.5065520394865,26.2535500850916,11.3310498250855));
#11175=CARTESIAN_POINT('Ctrl Pts',(-19.5672301992619,25.931798306063,11.0497998250855));
#11176=CARTESIAN_POINT('Ctrl Pts',(-19.8889860358136,24.8711154681011,10.7685498250855));
#11177=CARTESIAN_POINT('Ctrl Pts',(-19.1858154881714,24.0143125088581,10.4872998250855));
#11178=CARTESIAN_POINT('Ctrl Pts',(-18.0827552504337,24.1229408780555,10.2060498250855));
#11179=CARTESIAN_POINT('Ctrl Pts',(-17.5602368372596,25.1004978510396,9.92479982508548));
#11180=CARTESIAN_POINT('Ctrl Pts',(-18.0827746956949,26.0779661227699,9.64354982508546));
#11181=CARTESIAN_POINT('Ctrl Pts',(-19.1857665397851,26.1867290719232,9.36229982508548));
#11182=CARTESIAN_POINT('Ctrl Pts',(-19.8890898100541,25.3296760393435,9.08104982508546));
#11183=CARTESIAN_POINT('Ctrl Pts',(-19.5670178516484,24.2694882115909,8.79979982508548));
#11184=CARTESIAN_POINT('Ctrl Pts',(-18.5069841366212,23.9467388754675,8.51854982508546));
#11185=CARTESIAN_POINT('Ctrl Pts',(-17.6488539889194,24.6519402645264,8.23729982508548));
#11186=CARTESIAN_POINT('Ctrl Pts',(-17.741971675835,25.5674009602396,8.00292482508546));
#11187=CARTESIAN_POINT('Ctrl Pts',(-18.246320268237,26.0179629976208,7.81542482508548));
#11188=CARTESIAN_POINT('Ctrl Pts',(-18.5723996786931,26.1004782148047,7.72167482508547));
#11189=CARTESIAN_POINT('Ctrl Pts',(-18.7359120418715,26.1004782148047,7.67479982508547));
#11190=CARTESIAN_POINT('Ctrl Pts',(-18.7359120418715,26.1004782148047,16.6));
#11191=CARTESIAN_POINT('Ctrl Pts',(-18.899536659246,26.1004782148047,16.553125));
#11192=CARTESIAN_POINT('Ctrl Pts',(-19.2254952210856,26.0179991230989,16.459375));
#11193=CARTESIAN_POINT('Ctrl Pts',(-19.7300373474021,25.5673218790664,16.271875));
#11194=CARTESIAN_POINT('Ctrl Pts',(-19.8229633788124,24.6519659680192,16.0375));
#11195=CARTESIAN_POINT('Ctrl Pts',(-18.9648841528132,23.9466522306267,15.75625));
#11196=CARTESIAN_POINT('Ctrl Pts',(-17.9047456459512,24.2694552701876,15.475));
#11197=CARTESIAN_POINT('Ctrl Pts',(-17.5826797074142,25.3296825136249,15.19375));
#11198=CARTESIAN_POINT('Ctrl Pts',(-18.2860294065758,26.1867906898977,14.9125));
#11199=CARTESIAN_POINT('Ctrl Pts',(-19.389086573694,26.0780174976981,14.63125));
#11200=CARTESIAN_POINT('Ctrl Pts',(-19.9116498391532,25.1004985660911,14.35));
#11201=CARTESIAN_POINT('Ctrl Pts',(-19.3891045896494,24.1228877031823,14.06875));
#11202=CARTESIAN_POINT('Ctrl Pts',(-18.2859840561,24.0142539916667,13.7875));
#11203=CARTESIAN_POINT('Ctrl Pts',(-17.582775853732,24.8711029879984,13.50625));
#11204=CARTESIAN_POINT('Ctrl Pts',(-17.9045489079489,25.9318432698064,13.225));
#11205=CARTESIAN_POINT('Ctrl Pts',(-18.9652844651045,26.2536123707356,12.94375));
#11206=CARTESIAN_POINT('Ctrl Pts',(-19.8221414011456,25.5504093950162,12.6625));
#11207=CARTESIAN_POINT('Ctrl Pts',(-19.7134924282747,24.4472796581219,12.38125));
#11208=CARTESIAN_POINT('Ctrl Pts',(-18.7359120418715,23.9247523488297,12.1));
#11209=CARTESIAN_POINT('Ctrl Pts',(-17.7583316554683,24.4472796581219,11.81875));
#11210=CARTESIAN_POINT('Ctrl Pts',(-17.6496826825974,25.5504093950162,11.5375));
#11211=CARTESIAN_POINT('Ctrl Pts',(-18.5065396186384,26.2536123707357,11.25625));
#11212=CARTESIAN_POINT('Ctrl Pts',(-19.567275175794,25.9318432698063,10.975));
#11213=CARTESIAN_POINT('Ctrl Pts',(-19.8890482300109,24.8711029879984,10.69375));
#11214=CARTESIAN_POINT('Ctrl Pts',(-19.185840027643,24.0142539916666,10.4125));
#11215=CARTESIAN_POINT('Ctrl Pts',(-18.0827194940936,24.1228877031824,10.13125));
#11216=CARTESIAN_POINT('Ctrl Pts',(-17.5601742445898,25.1004985660911,9.85));
#11217=CARTESIAN_POINT('Ctrl Pts',(-18.082737510049,26.0780174976981,9.56875));
#11218=CARTESIAN_POINT('Ctrl Pts',(-19.1857946771672,26.1867906898977,9.2875));
#11219=CARTESIAN_POINT('Ctrl Pts',(-19.8891443763288,25.329682513625,9.00625));
#11220=CARTESIAN_POINT('Ctrl Pts',(-19.5670784377918,24.2694552701875,8.725));
#11221=CARTESIAN_POINT('Ctrl Pts',(-18.5069399309298,23.9466522306267,8.44375));
#11222=CARTESIAN_POINT('Ctrl Pts',(-17.6488607049306,24.6519659680192,8.16250000000001));
#11223=CARTESIAN_POINT('Ctrl Pts',(-17.7417867363409,25.5673218790663,7.928125));
#11224=CARTESIAN_POINT('Ctrl Pts',(-18.2463288626574,26.0179991230989,7.740625));
#11225=CARTESIAN_POINT('Ctrl Pts',(-18.572287424497,26.1004782148047,7.646875));
#11226=CARTESIAN_POINT('Ctrl Pts',(-18.7359120418715,26.1004782148047,7.6));
#11227=CARTESIAN_POINT('',(-18.7359120418715,26.1004782148047,7.6));
#11228=CARTESIAN_POINT('Ctrl Pts',(-18.7359120418715,26.1004782148047,16.6));
#11229=CARTESIAN_POINT('Ctrl Pts',(-18.899536659246,26.1004782148047,16.553125));
#11230=CARTESIAN_POINT('Ctrl Pts',(-19.2254952210856,26.0179991230989,16.459375));
#11231=CARTESIAN_POINT('Ctrl Pts',(-19.7300373474021,25.5673218790664,16.271875));
#11232=CARTESIAN_POINT('Ctrl Pts',(-19.8229633788124,24.6519659680192,16.0375));
#11233=CARTESIAN_POINT('Ctrl Pts',(-18.9648841528132,23.9466522306267,15.75625));
#11234=CARTESIAN_POINT('Ctrl Pts',(-17.9047456459512,24.2694552701876,15.475));
#11235=CARTESIAN_POINT('Ctrl Pts',(-17.5826797074142,25.3296825136249,15.19375));
#11236=CARTESIAN_POINT('Ctrl Pts',(-18.2860294065758,26.1867906898977,14.9125));
#11237=CARTESIAN_POINT('Ctrl Pts',(-19.389086573694,26.0780174976981,14.63125));
#11238=CARTESIAN_POINT('Ctrl Pts',(-19.9116498391532,25.1004985660911,14.35));
#11239=CARTESIAN_POINT('Ctrl Pts',(-19.3891045896494,24.1228877031823,14.06875));
#11240=CARTESIAN_POINT('Ctrl Pts',(-18.2859840561,24.0142539916667,13.7875));
#11241=CARTESIAN_POINT('Ctrl Pts',(-17.582775853732,24.8711029879984,13.50625));
#11242=CARTESIAN_POINT('Ctrl Pts',(-17.9045489079489,25.9318432698064,13.225));
#11243=CARTESIAN_POINT('Ctrl Pts',(-18.9652844651045,26.2536123707356,12.94375));
#11244=CARTESIAN_POINT('Ctrl Pts',(-19.8221414011456,25.5504093950162,12.6625));
#11245=CARTESIAN_POINT('Ctrl Pts',(-19.7134924282747,24.4472796581219,12.38125));
#11246=CARTESIAN_POINT('Ctrl Pts',(-18.7359120418715,23.9247523488297,12.1));
#11247=CARTESIAN_POINT('Ctrl Pts',(-17.7583316554683,24.4472796581219,11.81875));
#11248=CARTESIAN_POINT('Ctrl Pts',(-17.6496826825974,25.5504093950162,11.5375));
#11249=CARTESIAN_POINT('Ctrl Pts',(-18.5065396186384,26.2536123707357,11.25625));
#11250=CARTESIAN_POINT('Ctrl Pts',(-19.567275175794,25.9318432698063,10.975));
#11251=CARTESIAN_POINT('Ctrl Pts',(-19.8890482300109,24.8711029879984,10.69375));
#11252=CARTESIAN_POINT('Ctrl Pts',(-19.185840027643,24.0142539916666,10.4125));
#11253=CARTESIAN_POINT('Ctrl Pts',(-18.0827194940936,24.1228877031824,10.13125));
#11254=CARTESIAN_POINT('Ctrl Pts',(-17.5601742445898,25.1004985660911,9.85));
#11255=CARTESIAN_POINT('Ctrl Pts',(-18.082737510049,26.0780174976981,9.56875));
#11256=CARTESIAN_POINT('Ctrl Pts',(-19.1857946771672,26.1867906898977,9.2875));
#11257=CARTESIAN_POINT('Ctrl Pts',(-19.8891443763288,25.329682513625,9.00625));
#11258=CARTESIAN_POINT('Ctrl Pts',(-19.5670784377918,24.2694552701875,8.725));
#11259=CARTESIAN_POINT('Ctrl Pts',(-18.5069399309298,23.9466522306267,8.44375));
#11260=CARTESIAN_POINT('Ctrl Pts',(-17.6488607049306,24.6519659680192,8.16250000000001));
#11261=CARTESIAN_POINT('Ctrl Pts',(-17.7417867363409,25.5673218790663,7.928125));
#11262=CARTESIAN_POINT('Ctrl Pts',(-18.2463288626574,26.0179991230989,7.740625));
#11263=CARTESIAN_POINT('Ctrl Pts',(-18.572287424497,26.1004782148047,7.646875));
#11264=CARTESIAN_POINT('Ctrl Pts',(-18.7359120418715,26.1004782148047,7.6));
#11265=CARTESIAN_POINT('Origin',(-18.7359120418715,26.3504782148047,7.6));
#11266=CARTESIAN_POINT('Origin',(-18.7359120418715,26.3504782148047,7.6));
#11267=CARTESIAN_POINT('',(0.,0.,0.));
#11268=CARTESIAN_POINT('Origin',(-2.24952178519528,19.0640879581285,17.6));
#11269=CARTESIAN_POINT('',(-2.19952178519528,19.7140879581285,17.6));
#11270=CARTESIAN_POINT('Origin',(-2.19952178519528,19.0640879581285,17.6));
#11271=CARTESIAN_POINT('',(-2.29952178519528,19.8140879581285,17.6));
#11272=CARTESIAN_POINT('',(-2.24952178519528,19.7640879581285,17.6));
#11273=CARTESIAN_POINT('Origin',(-2.29952178519528,19.0640879581285,17.6));
#11274=CARTESIAN_POINT('Origin',(-7.59952178519528,19.0640879581285,17.6));
#11275=CARTESIAN_POINT('',(-7.49952178519528,19.8140879581285,17.6));
#11276=CARTESIAN_POINT('',(-7.59952178519528,19.8140879581285,17.6));
#11277=CARTESIAN_POINT('Origin',(-7.49952178519528,19.0640879581285,17.6));
#11278=CARTESIAN_POINT('Origin',(-2.19952178519528,19.0640879581285,17.6));
#11279=CARTESIAN_POINT('Origin',(-7.54952178519528,19.0640879581285,17.6));
#11280=CARTESIAN_POINT('',(-7.59952178519528,19.7140879581285,17.6));
#11281=CARTESIAN_POINT('',(-7.54952178519528,19.7640879581285,17.6));
#11282=CARTESIAN_POINT('Origin',(-7.59952178519528,19.0640879581285,17.6));
#11283=CARTESIAN_POINT('Origin',(-7.59952178519528,19.0640879581285,17.6));
#11284=CARTESIAN_POINT('',(0.,0.,0.));
#11285=CARTESIAN_POINT('Origin',(-24.6892783072069,25.1107216927931,9.2));
#11286=CARTESIAN_POINT('',(-27.2873545185602,25.1107216927931,7.7));
#11287=CARTESIAN_POINT('Origin',(-24.6892783072069,25.1107216927931,7.7));
#11288=CARTESIAN_POINT('',(-24.6892783072069,25.1107216927931,6.2));
#11289=CARTESIAN_POINT('Origin',(-24.6892783072069,25.1107216927931,9.2));
#11290=CARTESIAN_POINT('Origin',(-24.6892783072069,25.1107216927931,8.2));
#11291=CARTESIAN_POINT('',(-27.3468938358601,25.1107216927931,7.7));
#11292=CARTESIAN_POINT('Origin',(-24.6892783072069,25.1107216927931,7.7));
#11293=CARTESIAN_POINT('',(-27.8468938358601,25.1107216927931,8.2));
#11294=CARTESIAN_POINT('Origin',(-27.3468938358601,25.1107216927931,8.2));
#11295=CARTESIAN_POINT('Origin',(-24.6892783072069,25.1107216927931,8.2));
#11296=CARTESIAN_POINT('Origin',(-24.6892783072069,25.1107216927931,19.));
#11297=CARTESIAN_POINT('',(-27.8468938358601,25.1107216927931,18.5));
#11298=CARTESIAN_POINT('',(-27.8468938358601,25.1107216927931,19.));
#11299=CARTESIAN_POINT('Origin',(-24.6892783072069,25.1107216927931,18.5));
#11300=CARTESIAN_POINT('Origin',(-24.6892783072069,25.1107216927931,7.7));
#11301=CARTESIAN_POINT('Origin',(-24.6892783072069,23.3786708852242,19.));
#11302=CARTESIAN_POINT('',(-24.6892783072069,23.3786708852242,19.));
#11303=CARTESIAN_POINT('',(-26.1892783072069,24.2446962890086,19.));
#11304=CARTESIAN_POINT('',(-25.0642783072069,23.5951772361703,19.));
#11305=CARTESIAN_POINT('',(-24.6892783072069,23.3786708852242,18.));
#11306=CARTESIAN_POINT('',(-24.6892783072069,23.3786708852242,19.));
#11307=CARTESIAN_POINT('',(-26.1892783072069,24.2446962890086,18.));
#11308=CARTESIAN_POINT('',(-26.1892783072069,24.2446962890086,18.));
#11309=CARTESIAN_POINT('',(-26.1892783072069,24.2446962890086,19.));
#11310=CARTESIAN_POINT('Origin',(-23.1892783072069,24.2446962890086,19.));
#11311=CARTESIAN_POINT('',(-23.1892783072069,24.2446962890086,19.));
#11312=CARTESIAN_POINT('',(-23.5642783072069,24.0281899380625,19.));
#11313=CARTESIAN_POINT('',(-23.1892783072069,24.2446962890086,18.));
#11314=CARTESIAN_POINT('',(-23.1892783072069,24.2446962890086,19.));
#11315=CARTESIAN_POINT('',(-24.6892783072069,23.3786708852242,18.));
#11316=CARTESIAN_POINT('Origin',(-23.1892783072069,25.9767470965775,19.));
#11317=CARTESIAN_POINT('',(-23.1892783072069,25.9767470965775,19.));
#11318=CARTESIAN_POINT('',(-23.1892783072069,25.5437343946853,19.));
#11319=CARTESIAN_POINT('',(-23.1892783072069,25.9767470965775,18.));
#11320=CARTESIAN_POINT('',(-23.1892783072069,25.9767470965775,19.));
#11321=CARTESIAN_POINT('',(-23.1892783072069,24.2446962890086,18.));
#11322=CARTESIAN_POINT('Origin',(-24.6892783072069,26.842772500362,19.));
#11323=CARTESIAN_POINT('',(-24.6892783072069,26.842772500362,19.));
#11324=CARTESIAN_POINT('',(-24.3142783072069,26.6262661494158,19.));
#11325=CARTESIAN_POINT('',(-24.6892783072069,26.842772500362,18.));
#11326=CARTESIAN_POINT('',(-24.6892783072069,26.842772500362,19.));
#11327=CARTESIAN_POINT('',(-23.1892783072069,25.9767470965775,18.));
#11328=CARTESIAN_POINT('Origin',(-26.1892783072069,25.9767470965775,19.));
#11329=CARTESIAN_POINT('',(-26.1892783072069,25.9767470965775,19.));
#11330=CARTESIAN_POINT('',(-25.8142783072069,26.1932534475236,19.));
#11331=CARTESIAN_POINT('',(-26.1892783072069,25.9767470965775,18.));
#11332=CARTESIAN_POINT('',(-26.1892783072069,25.9767470965775,19.));
#11333=CARTESIAN_POINT('',(-24.6892783072069,26.842772500362,18.));
#11334=CARTESIAN_POINT('Origin',(-26.1892783072069,24.2446962890086,19.));
#11335=CARTESIAN_POINT('',(-26.1892783072069,24.6777089909009,19.));
#11336=CARTESIAN_POINT('',(-26.1892783072069,25.9767470965775,18.));
#11337=CARTESIAN_POINT('Origin',(-24.6892783072069,25.1107216927931,18.));
#11338=CARTESIAN_POINT('Origin',(-24.6892783072069,25.1107216927931,18.75));
#11339=CARTESIAN_POINT('',(-27.3468938358601,25.1107216927931,19.));
#11340=CARTESIAN_POINT('Origin',(-24.6892783072069,25.1107216927931,19.));
#11341=CARTESIAN_POINT('',(-27.5968938358601,25.1107216927931,18.75));
#11342=CARTESIAN_POINT('Origin',(-24.6892783072069,25.1107216927931,19.));
#11343=CARTESIAN_POINT('',(0.,0.,0.));
#11344=CARTESIAN_POINT('',(0.,0.,0.));
#11345=CARTESIAN_POINT('',(0.,0.,0.));
#11346=CARTESIAN_POINT('',(0.,0.,0.));
#11347=CARTESIAN_POINT('',(0.,0.,0.));
#11348=CARTESIAN_POINT('',(0.,0.,0.));
#11349=CARTESIAN_POINT('',(0.,0.,0.));
#11350=CARTESIAN_POINT('',(0.,0.,0.));
#11351=CARTESIAN_POINT('',(0.,0.,0.));
#11352=CARTESIAN_POINT('',(0.,0.,0.));
#11353=CARTESIAN_POINT('',(0.,0.,0.));
#11354=CARTESIAN_POINT('',(0.,0.,0.));
#11355=CARTESIAN_POINT('',(0.,0.,0.));
#11356=UNCERTAINTY_MEASURE_WITH_UNIT(LENGTH_MEASURE(0.01),#11386,
'DISTANCE_ACCURACY_VALUE',
'Maximum model space distance between geometric entities at asserted c
onnectivities');
#11357=UNCERTAINTY_MEASURE_WITH_UNIT(LENGTH_MEASURE(0.01),#11386,
'DISTANCE_ACCURACY_VALUE',
'Maximum model space distance between geometric entities at asserted c
onnectivities');
#11358=UNCERTAINTY_MEASURE_WITH_UNIT(LENGTH_MEASURE(0.01),#11386,
'DISTANCE_ACCURACY_VALUE',
'Maximum model space distance between geometric entities at asserted c
onnectivities');
#11359=UNCERTAINTY_MEASURE_WITH_UNIT(LENGTH_MEASURE(0.01),#11386,
'DISTANCE_ACCURACY_VALUE',
'Maximum model space distance between geometric entities at asserted c
onnectivities');
#11360=UNCERTAINTY_MEASURE_WITH_UNIT(LENGTH_MEASURE(0.01),#11386,
'DISTANCE_ACCURACY_VALUE',
'Maximum model space distance between geometric entities at asserted c
onnectivities');
#11361=UNCERTAINTY_MEASURE_WITH_UNIT(LENGTH_MEASURE(0.01),#11386,
'DISTANCE_ACCURACY_VALUE',
'Maximum model space distance between geometric entities at asserted c
onnectivities');
#11362=UNCERTAINTY_MEASURE_WITH_UNIT(LENGTH_MEASURE(0.01),#11386,
'DISTANCE_ACCURACY_VALUE',
'Maximum model space distance between geometric entities at asserted c
onnectivities');
#11363=UNCERTAINTY_MEASURE_WITH_UNIT(LENGTH_MEASURE(0.01),#11386,
'DISTANCE_ACCURACY_VALUE',
'Maximum model space distance between geometric entities at asserted c
onnectivities');
#11364=UNCERTAINTY_MEASURE_WITH_UNIT(LENGTH_MEASURE(0.01),#11386,
'DISTANCE_ACCURACY_VALUE',
'Maximum model space distance between geometric entities at asserted c
onnectivities');
#11365=UNCERTAINTY_MEASURE_WITH_UNIT(LENGTH_MEASURE(0.01),#11386,
'DISTANCE_ACCURACY_VALUE',
'Maximum model space distance between geometric entities at asserted c
onnectivities');
#11366=UNCERTAINTY_MEASURE_WITH_UNIT(LENGTH_MEASURE(0.01),#11386,
'DISTANCE_ACCURACY_VALUE',
'Maximum model space distance between geometric entities at asserted c
onnectivities');
#11367=UNCERTAINTY_MEASURE_WITH_UNIT(LENGTH_MEASURE(0.01),#11386,
'DISTANCE_ACCURACY_VALUE',
'Maximum model space distance between geometric entities at asserted c
onnectivities');
#11368=UNCERTAINTY_MEASURE_WITH_UNIT(LENGTH_MEASURE(0.01),#11386,
'DISTANCE_ACCURACY_VALUE',
'Maximum model space distance between geometric entities at asserted c
onnectivities');
#11369=UNCERTAINTY_MEASURE_WITH_UNIT(LENGTH_MEASURE(0.01),#11386,
'DISTANCE_ACCURACY_VALUE',
'Maximum model space distance between geometric entities at asserted c
onnectivities');
#11370=UNCERTAINTY_MEASURE_WITH_UNIT(LENGTH_MEASURE(0.01),#11386,
'DISTANCE_ACCURACY_VALUE',
'Maximum model space distance between geometric entities at asserted c
onnectivities');
#11371=(
GEOMETRIC_REPRESENTATION_CONTEXT(3)
GLOBAL_UNCERTAINTY_ASSIGNED_CONTEXT((#11356))
GLOBAL_UNIT_ASSIGNED_CONTEXT((#11386,#11388,#11389))
REPRESENTATION_CONTEXT('','3D')
);
#11372=(
GEOMETRIC_REPRESENTATION_CONTEXT(3)
GLOBAL_UNCERTAINTY_ASSIGNED_CONTEXT((#11357))
GLOBAL_UNIT_ASSIGNED_CONTEXT((#11386,#11388,#11389))
REPRESENTATION_CONTEXT('','3D')
);
#11373=(
GEOMETRIC_REPRESENTATION_CONTEXT(3)
GLOBAL_UNCERTAINTY_ASSIGNED_CONTEXT((#11358))
GLOBAL_UNIT_ASSIGNED_CONTEXT((#11386,#11388,#11389))
REPRESENTATION_CONTEXT('','3D')
);
#11374=(
GEOMETRIC_REPRESENTATION_CONTEXT(3)
GLOBAL_UNCERTAINTY_ASSIGNED_CONTEXT((#11359))
GLOBAL_UNIT_ASSIGNED_CONTEXT((#11386,#11388,#11389))
REPRESENTATION_CONTEXT('','3D')
);
#11375=(
GEOMETRIC_REPRESENTATION_CONTEXT(3)
GLOBAL_UNCERTAINTY_ASSIGNED_CONTEXT((#11360))
GLOBAL_UNIT_ASSIGNED_CONTEXT((#11386,#11388,#11389))
REPRESENTATION_CONTEXT('','3D')
);
#11376=(
GEOMETRIC_REPRESENTATION_CONTEXT(3)
GLOBAL_UNCERTAINTY_ASSIGNED_CONTEXT((#11361))
GLOBAL_UNIT_ASSIGNED_CONTEXT((#11386,#11388,#11389))
REPRESENTATION_CONTEXT('','3D')
);
#11377=(
GEOMETRIC_REPRESENTATION_CONTEXT(3)
GLOBAL_UNCERTAINTY_ASSIGNED_CONTEXT((#11362))
GLOBAL_UNIT_ASSIGNED_CONTEXT((#11386,#11388,#11389))
REPRESENTATION_CONTEXT('','3D')
);
#11378=(
GEOMETRIC_REPRESENTATION_CONTEXT(3)
GLOBAL_UNCERTAINTY_ASSIGNED_CONTEXT((#11363))
GLOBAL_UNIT_ASSIGNED_CONTEXT((#11386,#11388,#11389))
REPRESENTATION_CONTEXT('','3D')
);
#11379=(
GEOMETRIC_REPRESENTATION_CONTEXT(3)
GLOBAL_UNCERTAINTY_ASSIGNED_CONTEXT((#11364))
GLOBAL_UNIT_ASSIGNED_CONTEXT((#11386,#11388,#11389))
REPRESENTATION_CONTEXT('','3D')
);
#11380=(
GEOMETRIC_REPRESENTATION_CONTEXT(3)
GLOBAL_UNCERTAINTY_ASSIGNED_CONTEXT((#11365))
GLOBAL_UNIT_ASSIGNED_CONTEXT((#11386,#11388,#11389))
REPRESENTATION_CONTEXT('','3D')
);
#11381=(
GEOMETRIC_REPRESENTATION_CONTEXT(3)
GLOBAL_UNCERTAINTY_ASSIGNED_CONTEXT((#11366))
GLOBAL_UNIT_ASSIGNED_CONTEXT((#11386,#11388,#11389))
REPRESENTATION_CONTEXT('','3D')
);
#11382=(
GEOMETRIC_REPRESENTATION_CONTEXT(3)
GLOBAL_UNCERTAINTY_ASSIGNED_CONTEXT((#11367))
GLOBAL_UNIT_ASSIGNED_CONTEXT((#11386,#11388,#11389))
REPRESENTATION_CONTEXT('','3D')
);
#11383=(
GEOMETRIC_REPRESENTATION_CONTEXT(3)
GLOBAL_UNCERTAINTY_ASSIGNED_CONTEXT((#11368))
GLOBAL_UNIT_ASSIGNED_CONTEXT((#11386,#11388,#11389))
REPRESENTATION_CONTEXT('','3D')
);
#11384=(
GEOMETRIC_REPRESENTATION_CONTEXT(3)
GLOBAL_UNCERTAINTY_ASSIGNED_CONTEXT((#11369))
GLOBAL_UNIT_ASSIGNED_CONTEXT((#11386,#11388,#11389))
REPRESENTATION_CONTEXT('','3D')
);
#11385=(
GEOMETRIC_REPRESENTATION_CONTEXT(3)
GLOBAL_UNCERTAINTY_ASSIGNED_CONTEXT((#11370))
GLOBAL_UNIT_ASSIGNED_CONTEXT((#11386,#11388,#11389))
REPRESENTATION_CONTEXT('','3D')
);
#11386=(
LENGTH_UNIT()
NAMED_UNIT(*)
SI_UNIT(.MILLI.,.METRE.)
);
#11387=(
LENGTH_UNIT()
NAMED_UNIT(*)
SI_UNIT($,.METRE.)
);
#11388=(
NAMED_UNIT(*)
PLANE_ANGLE_UNIT()
SI_UNIT($,.RADIAN.)
);
#11389=(
NAMED_UNIT(*)
SI_UNIT($,.STERADIAN.)
SOLID_ANGLE_UNIT()
);
#11390=SHAPE_DEFINITION_REPRESENTATION(#11404,#11431);
#11391=SHAPE_DEFINITION_REPRESENTATION(#11405,#11432);
#11392=SHAPE_DEFINITION_REPRESENTATION(#11406,#11433);
#11393=SHAPE_DEFINITION_REPRESENTATION(#11407,#11434);
#11394=SHAPE_DEFINITION_REPRESENTATION(#11408,#11435);
#11395=SHAPE_DEFINITION_REPRESENTATION(#11409,#11436);
#11396=SHAPE_DEFINITION_REPRESENTATION(#11410,#11437);
#11397=SHAPE_DEFINITION_REPRESENTATION(#11411,#11438);
#11398=SHAPE_DEFINITION_REPRESENTATION(#11412,#11439);
#11399=SHAPE_DEFINITION_REPRESENTATION(#11413,#11440);
#11400=SHAPE_DEFINITION_REPRESENTATION(#11414,#11441);
#11401=SHAPE_DEFINITION_REPRESENTATION(#11415,#11442);
#11402=SHAPE_DEFINITION_REPRESENTATION(#11416,#11443);
#11403=SHAPE_DEFINITION_REPRESENTATION(#11417,#11444);
#11404=PRODUCT_DEFINITION_SHAPE('',$,#11446);
#11405=PRODUCT_DEFINITION_SHAPE('',$,#11447);
#11406=PRODUCT_DEFINITION_SHAPE('',$,#11448);
#11407=PRODUCT_DEFINITION_SHAPE('',$,#11449);
#11408=PRODUCT_DEFINITION_SHAPE('',$,#11450);
#11409=PRODUCT_DEFINITION_SHAPE('',$,#11451);
#11410=PRODUCT_DEFINITION_SHAPE('',$,#11452);
#11411=PRODUCT_DEFINITION_SHAPE('',$,#11453);
#11412=PRODUCT_DEFINITION_SHAPE('',$,#11454);
#11413=PRODUCT_DEFINITION_SHAPE('',$,#11455);
#11414=PRODUCT_DEFINITION_SHAPE('',$,#11456);
#11415=PRODUCT_DEFINITION_SHAPE('',$,#11457);
#11416=PRODUCT_DEFINITION_SHAPE('',$,#11458);
#11417=PRODUCT_DEFINITION_SHAPE('',$,#11459);
#11418=PRODUCT_DEFINITION_SHAPE($,$,#50);
#11419=PRODUCT_DEFINITION_SHAPE($,$,#51);
#11420=PRODUCT_DEFINITION_SHAPE($,$,#52);
#11421=PRODUCT_DEFINITION_SHAPE($,$,#53);
#11422=PRODUCT_DEFINITION_SHAPE($,$,#54);
#11423=PRODUCT_DEFINITION_SHAPE($,$,#55);
#11424=PRODUCT_DEFINITION_SHAPE($,$,#56);
#11425=PRODUCT_DEFINITION_SHAPE($,$,#57);
#11426=PRODUCT_DEFINITION_SHAPE($,$,#58);
#11427=PRODUCT_DEFINITION_SHAPE($,$,#59);
#11428=PRODUCT_DEFINITION_SHAPE($,$,#60);
#11429=PRODUCT_DEFINITION_SHAPE($,$,#61);
#11430=PRODUCT_DEFINITION_SHAPE($,$,#62);
#11431=SHAPE_REPRESENTATION('',(#5499,#6097,#6098,#6099,#6100,#6101,#6102,
#6103,#6104,#6105,#6106,#6107,#6108,#6109),#11371);
#11432=SHAPE_REPRESENTATION('',(#5500),#11372);
#11433=SHAPE_REPRESENTATION('',(#5779),#11373);
#11434=SHAPE_REPRESENTATION('',(#5789),#11374);
#11435=SHAPE_REPRESENTATION('',(#5796),#11375);
#11436=SHAPE_REPRESENTATION('',(#5817),#11376);
#11437=SHAPE_REPRESENTATION('',(#6004),#11377);
#11438=SHAPE_REPRESENTATION('',(#6014),#11378);
#11439=SHAPE_REPRESENTATION('',(#6035),#11379);
#11440=SHAPE_REPRESENTATION('',(#6042),#11380);
#11441=SHAPE_REPRESENTATION('',(#6049),#11381);
#11442=SHAPE_REPRESENTATION('',(#6059),#11382);
#11443=SHAPE_REPRESENTATION('',(#6066),#11383);
#11444=SHAPE_REPRESENTATION('',(#6076),#11384);
#11445=PRODUCT_DEFINITION_CONTEXT('part definition',#11489,'design');
#11446=PRODUCT_DEFINITION('MAS-280','MAS-280',#11460,#11445);
#11447=PRODUCT_DEFINITION('Top_Block','Top_Block',#11461,#11445);
#11448=PRODUCT_DEFINITION('Pin_01','Pin_01',#11462,#11445);
#11449=PRODUCT_DEFINITION('Spring_01','Spring_01',#11463,#11445);
#11450=PRODUCT_DEFINITION('Ball_Screw_01','Ball_Screw_01',#11464,#11445);
#11451=PRODUCT_DEFINITION('Bottom_Block','Bottom_Block',#11465,#11445);
#11452=PRODUCT_DEFINITION('Pin_04','Pin_04',#11466,#11445);
#11453=PRODUCT_DEFINITION('Ball_Screw_02','Ball_Screw_02',#11467,#11445);
#11454=PRODUCT_DEFINITION('Spring_04','Spring_04',#11468,#11445);
#11455=PRODUCT_DEFINITION('Spring_02','Spring_02',#11469,#11445);
#11456=PRODUCT_DEFINITION('Pin_03','Pin_03',#11470,#11445);
#11457=PRODUCT_DEFINITION('Spring_03','Spring_03',#11471,#11445);
#11458=PRODUCT_DEFINITION('Pin_02','Pin_02',#11472,#11445);
#11459=PRODUCT_DEFINITION('Ball_Screw_03','Ball_Screw_03',#11473,#11445);
#11460=PRODUCT_DEFINITION_FORMATION('',$,#11491);
#11461=PRODUCT_DEFINITION_FORMATION('',$,#11492);
#11462=PRODUCT_DEFINITION_FORMATION('',$,#11493);
#11463=PRODUCT_DEFINITION_FORMATION('',$,#11494);
#11464=PRODUCT_DEFINITION_FORMATION('',$,#11495);
#11465=PRODUCT_DEFINITION_FORMATION('',$,#11496);
#11466=PRODUCT_DEFINITION_FORMATION('',$,#11497);
#11467=PRODUCT_DEFINITION_FORMATION('',$,#11498);
#11468=PRODUCT_DEFINITION_FORMATION('',$,#11499);
#11469=PRODUCT_DEFINITION_FORMATION('',$,#11500);
#11470=PRODUCT_DEFINITION_FORMATION('',$,#11501);
#11471=PRODUCT_DEFINITION_FORMATION('',$,#11502);
#11472=PRODUCT_DEFINITION_FORMATION('',$,#11503);
#11473=PRODUCT_DEFINITION_FORMATION('',$,#11504);
#11474=PRODUCT_RELATED_PRODUCT_CATEGORY('MAS-280','MAS-280',(#11491));
#11475=PRODUCT_RELATED_PRODUCT_CATEGORY('Top_Block','Top_Block',(#11492));
#11476=PRODUCT_RELATED_PRODUCT_CATEGORY('Pin_01','Pin_01',(#11493));
#11477=PRODUCT_RELATED_PRODUCT_CATEGORY('Spring_01','Spring_01',(#11494));
#11478=PRODUCT_RELATED_PRODUCT_CATEGORY('Ball_Screw_01','Ball_Screw_01',
(#11495));
#11479=PRODUCT_RELATED_PRODUCT_CATEGORY('Bottom_Block','Bottom_Block',(#11496));
#11480=PRODUCT_RELATED_PRODUCT_CATEGORY('Pin_04','Pin_04',(#11497));
#11481=PRODUCT_RELATED_PRODUCT_CATEGORY('Ball_Screw_02','Ball_Screw_02',
(#11498));
#11482=PRODUCT_RELATED_PRODUCT_CATEGORY('Spring_04','Spring_04',(#11499));
#11483=PRODUCT_RELATED_PRODUCT_CATEGORY('Spring_02','Spring_02',(#11500));
#11484=PRODUCT_RELATED_PRODUCT_CATEGORY('Pin_03','Pin_03',(#11501));
#11485=PRODUCT_RELATED_PRODUCT_CATEGORY('Spring_03','Spring_03',(#11502));
#11486=PRODUCT_RELATED_PRODUCT_CATEGORY('Pin_02','Pin_02',(#11503));
#11487=PRODUCT_RELATED_PRODUCT_CATEGORY('Ball_Screw_03','Ball_Screw_03',
(#11504));
#11488=APPLICATION_PROTOCOL_DEFINITION('international standard',
'automotive_design',2009,#11489);
#11489=APPLICATION_CONTEXT(
'Core Data for Automotive Mechanical Design Process');
#11490=PRODUCT_CONTEXT('part definition',#11489,'mechanical');
#11491=PRODUCT('MAS-280','MAS-280',$,(#11490));
#11492=PRODUCT('Top_Block','Top_Block',$,(#11490));
#11493=PRODUCT('Pin_01','Pin_01',$,(#11490));
#11494=PRODUCT('Spring_01','Spring_01',$,(#11490));
#11495=PRODUCT('Ball_Screw_01','Ball_Screw_01',$,(#11490));
#11496=PRODUCT('Bottom_Block','Bottom_Block',$,(#11490));
#11497=PRODUCT('Pin_04','Pin_04',$,(#11490));
#11498=PRODUCT('Ball_Screw_02','Ball_Screw_02',$,(#11490));
#11499=PRODUCT('Spring_04','Spring_04',$,(#11490));
#11500=PRODUCT('Spring_02','Spring_02',$,(#11490));
#11501=PRODUCT('Pin_03','Pin_03',$,(#11490));
#11502=PRODUCT('Spring_03','Spring_03',$,(#11490));
#11503=PRODUCT('Pin_02','Pin_02',$,(#11490));
#11504=PRODUCT('Ball_Screw_03','Ball_Screw_03',$,(#11490));
#11505=PRESENTATION_STYLE_ASSIGNMENT((#11510));
#11506=PRESENTATION_STYLE_ASSIGNMENT((#11511));
#11507=PRESENTATION_STYLE_ASSIGNMENT((#11512));
#11508=PRESENTATION_STYLE_ASSIGNMENT((#11513));
#11509=PRESENTATION_STYLE_ASSIGNMENT((#11514));
#11510=SURFACE_STYLE_USAGE(.BOTH.,#11515);
#11511=SURFACE_STYLE_USAGE(.BOTH.,#11516);
#11512=SURFACE_STYLE_USAGE(.BOTH.,#11517);
#11513=SURFACE_STYLE_USAGE(.BOTH.,#11518);
#11514=SURFACE_STYLE_USAGE(.BOTH.,#11519);
#11515=SURFACE_SIDE_STYLE('',(#11520));
#11516=SURFACE_SIDE_STYLE('',(#11521));
#11517=SURFACE_SIDE_STYLE('',(#11522));
#11518=SURFACE_SIDE_STYLE('',(#11523));
#11519=SURFACE_SIDE_STYLE('',(#11524));
#11520=SURFACE_STYLE_FILL_AREA(#11525);
#11521=SURFACE_STYLE_FILL_AREA(#11526);
#11522=SURFACE_STYLE_FILL_AREA(#11527);
#11523=SURFACE_STYLE_FILL_AREA(#11528);
#11524=SURFACE_STYLE_FILL_AREA(#11529);
#11525=FILL_AREA_STYLE('Steel - Satin',(#11530));
#11526=FILL_AREA_STYLE('Opaque(64,64,64)',(#11531));
#11527=FILL_AREA_STYLE('Aluminum - Polished',(#11532));
#11528=FILL_AREA_STYLE('Steel - Satin (1)',(#11533));
#11529=FILL_AREA_STYLE('Opaque(255,242,232)',(#11534));
#11530=FILL_AREA_STYLE_COLOUR('Steel - Satin',#11535);
#11531=FILL_AREA_STYLE_COLOUR('Opaque(64,64,64)',#11536);
#11532=FILL_AREA_STYLE_COLOUR('Aluminum - Polished',#11537);
#11533=FILL_AREA_STYLE_COLOUR('Steel - Satin (1)',#11538);
#11534=FILL_AREA_STYLE_COLOUR('Opaque(255,242,232)',#11539);
#11535=COLOUR_RGB('Steel - Satin',0.627450980392157,0.627450980392157,0.627450980392157);
#11536=COLOUR_RGB('Opaque(64,64,64)',0.250980392156863,0.250980392156863,
0.250980392156863);
#11537=COLOUR_RGB('Aluminum - Polished',0.96078431372549,0.96078431372549,
0.964705882352941);
#11538=COLOUR_RGB('Steel - Satin (1)',0.627450980392157,0.627450980392157,
0.627450980392157);
#11539=COLOUR_RGB('Opaque(255,242,232)',1.,0.949019607843137,0.909803921568627);
#11540=COLOUR_RGB('Dark Blue',0.08,0.2,0.34);
#11541=FILL_AREA_STYLE_COLOUR('',#11540);
#11542=FILL_AREA_STYLE('',(#11541));
#11543=SURFACE_STYLE_FILL_AREA(#11542);
#11544=SURFACE_SIDE_STYLE('',(#11543));
#11545=SURFACE_STYLE_USAGE(.BOTH.,#11544);
#11546=PRESENTATION_STYLE_ASSIGNMENT((#11545));
#11547=COLOUR_RGB('Light Blue',0.38,0.62,0.78);
#11548=FILL_AREA_STYLE_COLOUR('',#11547);
#11549=FILL_AREA_STYLE('',(#11548));
#11550=SURFACE_STYLE_FILL_AREA(#11549);
#11551=SURFACE_SIDE_STYLE('',(#11550));
#11552=SURFACE_STYLE_USAGE(.BOTH.,#11551);
#11553=PRESENTATION_STYLE_ASSIGNMENT((#11552));
#11554=COLOUR_RGB('Sky Blue',0.24,0.69,0.87);
#11555=FILL_AREA_STYLE_COLOUR('',#11554);
#11556=FILL_AREA_STYLE('',(#11555));
#11557=SURFACE_STYLE_FILL_AREA(#11556);
#11558=SURFACE_SIDE_STYLE('',(#11557));
#11559=SURFACE_STYLE_USAGE(.BOTH.,#11558);
#11560=PRESENTATION_STYLE_ASSIGNMENT((#11559));
#11561=COLOUR_RGB('Grey',0.48,0.52,0.57);
#11562=FILL_AREA_STYLE_COLOUR('',#11561);
#11563=FILL_AREA_STYLE('',(#11562));
#11564=SURFACE_STYLE_FILL_AREA(#11563);
#11565=SURFACE_SIDE_STYLE('',(#11564));
#11566=SURFACE_STYLE_USAGE(.BOTH.,#11565);
#11567=PRESENTATION_STYLE_ASSIGNMENT((#11566));
#11568=COLOUR_RGB('Black',0.12,0.14,0.17);
#11569=FILL_AREA_STYLE_COLOUR('',#11568);
#11570=FILL_AREA_STYLE('',(#11569));
#11571=SURFACE_STYLE_FILL_AREA(#11570);
#11572=SURFACE_SIDE_STYLE('',(#11571));
#11573=SURFACE_STYLE_USAGE(.BOTH.,#11572);
#11574=PRESENTATION_STYLE_ASSIGNMENT((#11573));
#11575=COLOUR_RGB('Off White',0.89,0.88,0.83);
#11576=FILL_AREA_STYLE_COLOUR('',#11575);
#11577=FILL_AREA_STYLE('',(#11576));
#11578=SURFACE_STYLE_FILL_AREA(#11577);
#11579=SURFACE_SIDE_STYLE('',(#11578));
#11580=SURFACE_STYLE_USAGE(.BOTH.,#11579);
#11581=PRESENTATION_STYLE_ASSIGNMENT((#11580));
ENDSEC;
END-ISO-10303-21;
